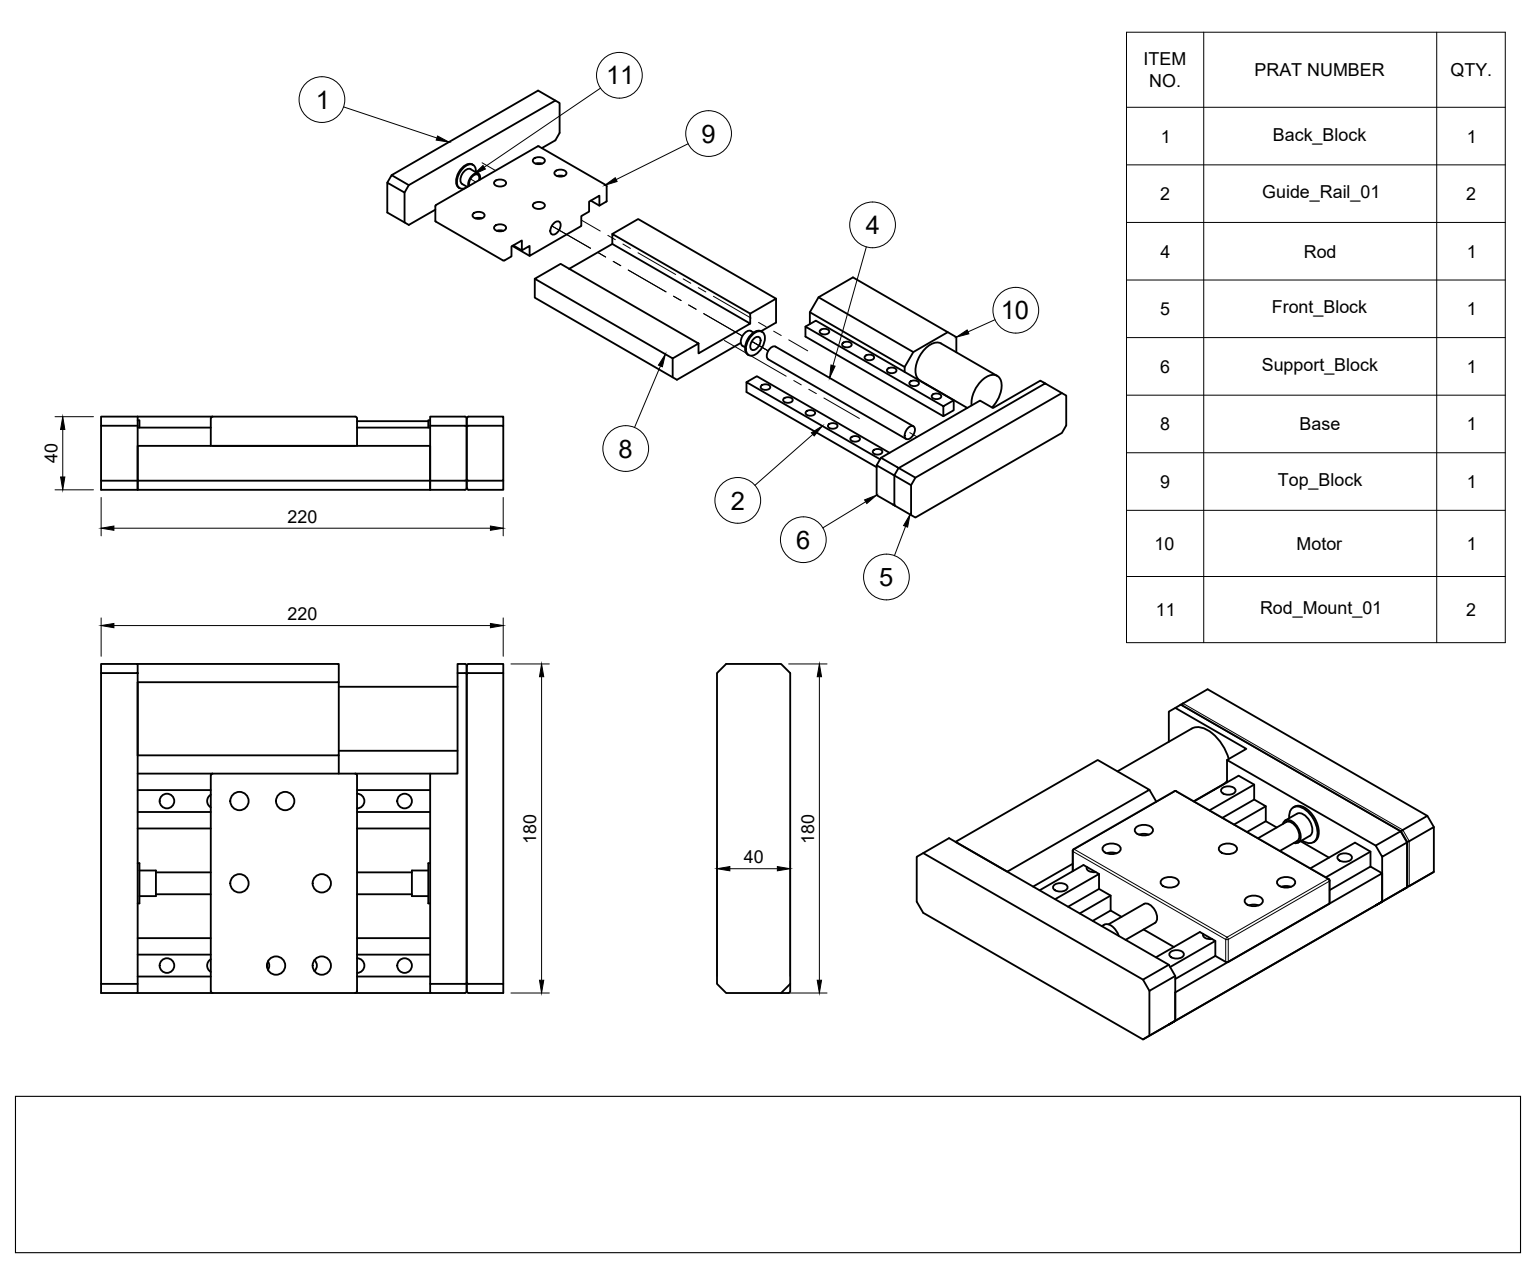
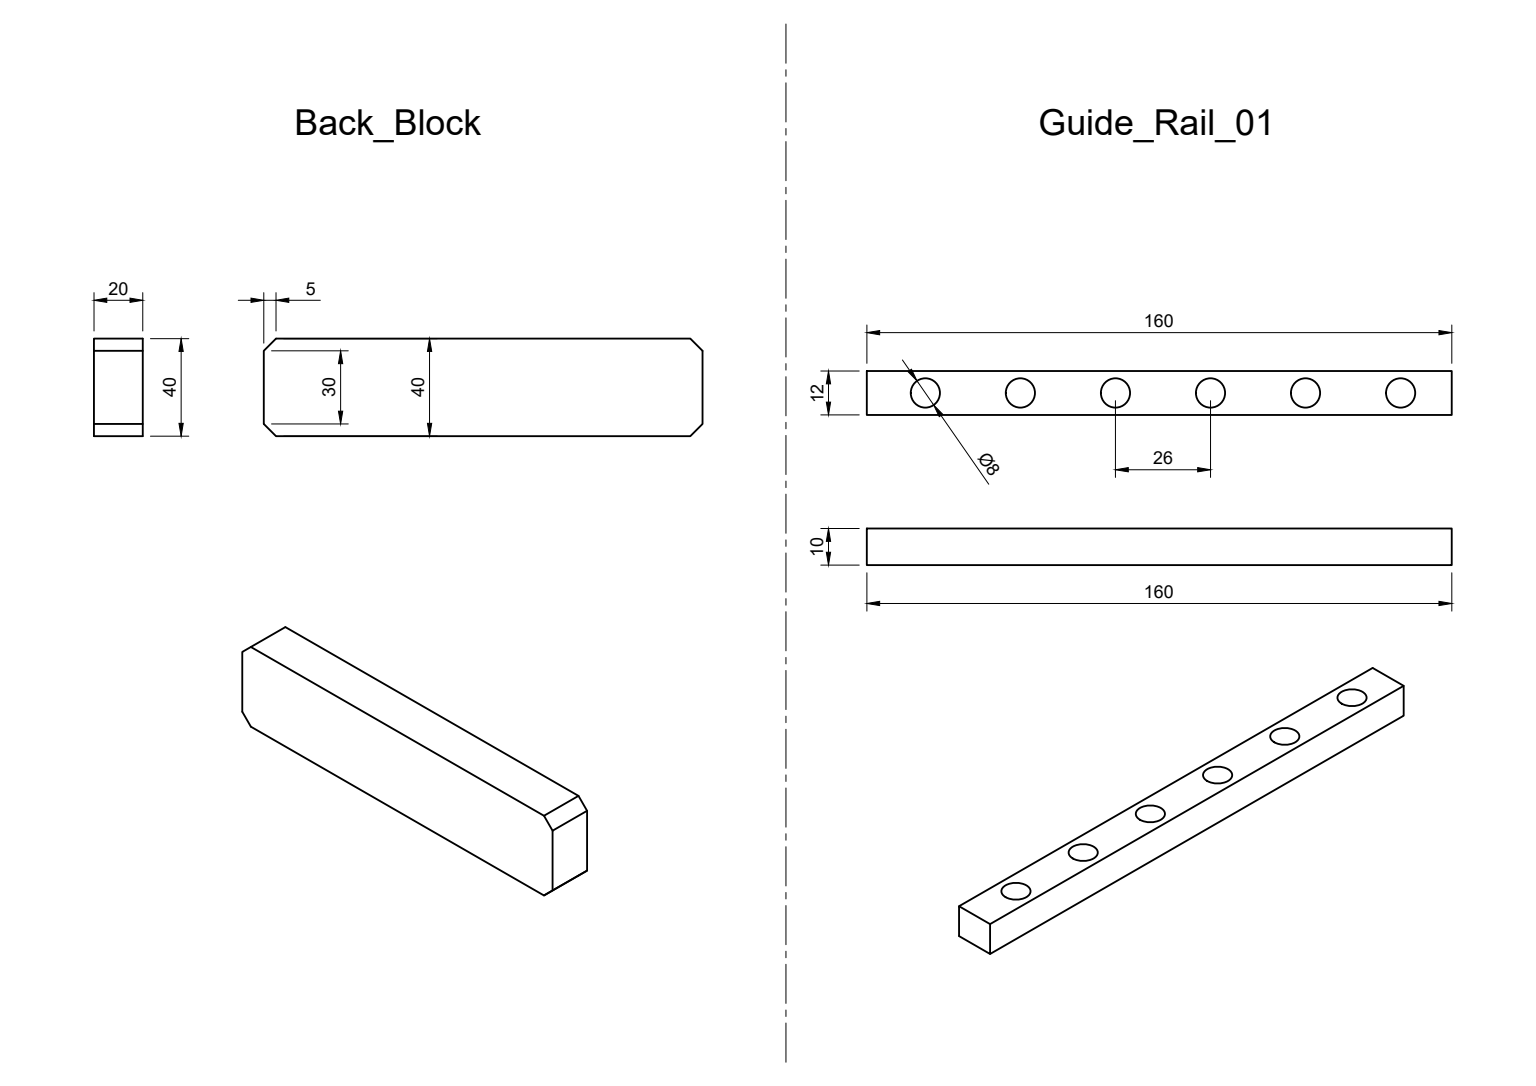
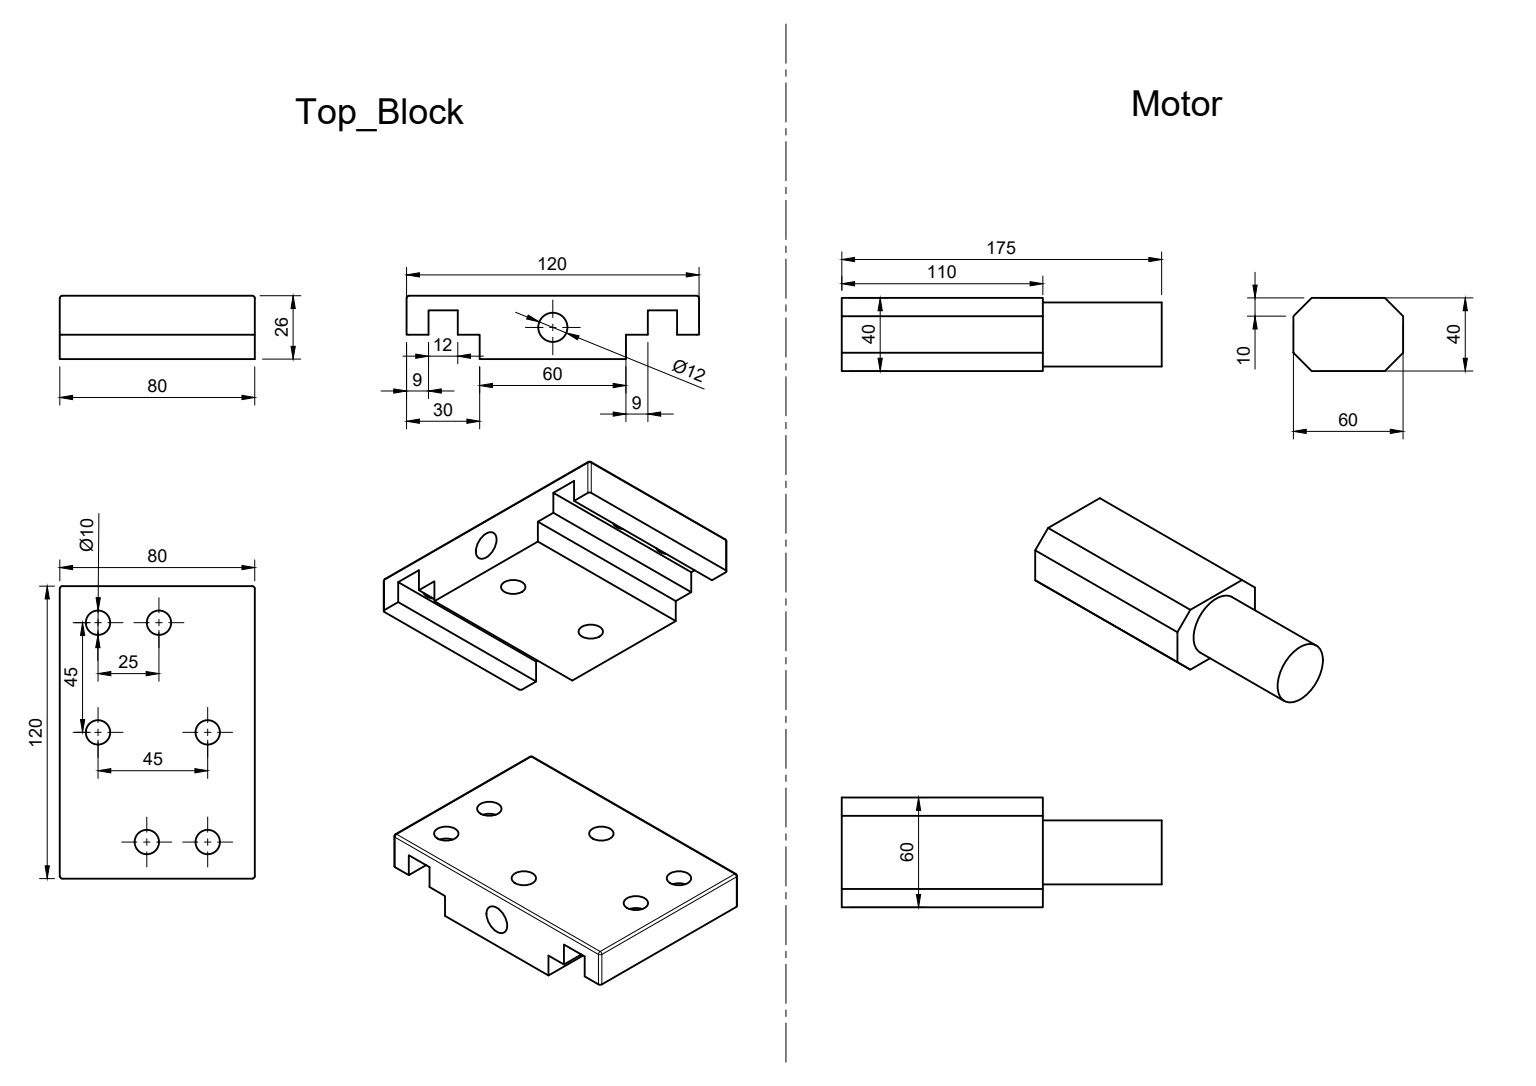
ISO-10303-21;
HEADER;
/* Generated by software containing ST-Developer
 * from STEP Tools, Inc. (www.steptools.com) 
 */

FILE_DESCRIPTION(
/* description */ (''),
/* implementation_level */ '2;1');

FILE_NAME(
/* name */ 'MAS-269',
/* time_stamp */ '2026-10-19T02:00:06+06:00',
/* author */ (''),
/* organization */ (''),
/* preprocessor_version */ 'ST-DEVELOPER v20.2',
/* originating_system */ 'Autodesk Translation Framework v15.15.0.0',
/* authorisation */ '');

FILE_SCHEMA (('AUTOMOTIVE_DESIGN { 1 0 10303 214 3 1 1 }'));
ENDSEC;

DATA;
#10=MECHANICAL_DESIGN_GEOMETRIC_PRESENTATION_REPRESENTATION('',(#105,#106,
#107,#108,#109,#110,#111,#112,#113,#114,#115),#4833);
#11=ITEM_DEFINED_TRANSFORMATION($,$,#2821,#3079);
#12=ITEM_DEFINED_TRANSFORMATION($,$,#2852,#3080);
#13=ITEM_DEFINED_TRANSFORMATION($,$,#2883,#3081);
#14=ITEM_DEFINED_TRANSFORMATION($,$,#2889,#3082);
#15=ITEM_DEFINED_TRANSFORMATION($,$,#2916,#3083);
#16=ITEM_DEFINED_TRANSFORMATION($,$,#2945,#3084);
#17=ITEM_DEFINED_TRANSFORMATION($,$,#2958,#3085);
#18=ITEM_DEFINED_TRANSFORMATION($,$,#2970,#3086);
#19=ITEM_DEFINED_TRANSFORMATION($,$,#3040,#3087);
#20=ITEM_DEFINED_TRANSFORMATION($,$,#3055,#3088);
#21=ITEM_DEFINED_TRANSFORMATION($,$,#3068,#3089);
#22=(
REPRESENTATION_RELATIONSHIP($,$,#4874,#4873)
REPRESENTATION_RELATIONSHIP_WITH_TRANSFORMATION(#11)
SHAPE_REPRESENTATION_RELATIONSHIP()
);
#23=(
REPRESENTATION_RELATIONSHIP($,$,#4875,#4873)
REPRESENTATION_RELATIONSHIP_WITH_TRANSFORMATION(#12)
SHAPE_REPRESENTATION_RELATIONSHIP()
);
#24=(
REPRESENTATION_RELATIONSHIP($,$,#4876,#4873)
REPRESENTATION_RELATIONSHIP_WITH_TRANSFORMATION(#13)
SHAPE_REPRESENTATION_RELATIONSHIP()
);
#25=(
REPRESENTATION_RELATIONSHIP($,$,#4877,#4873)
REPRESENTATION_RELATIONSHIP_WITH_TRANSFORMATION(#14)
SHAPE_REPRESENTATION_RELATIONSHIP()
);
#26=(
REPRESENTATION_RELATIONSHIP($,$,#4878,#4873)
REPRESENTATION_RELATIONSHIP_WITH_TRANSFORMATION(#15)
SHAPE_REPRESENTATION_RELATIONSHIP()
);
#27=(
REPRESENTATION_RELATIONSHIP($,$,#4879,#4873)
REPRESENTATION_RELATIONSHIP_WITH_TRANSFORMATION(#16)
SHAPE_REPRESENTATION_RELATIONSHIP()
);
#28=(
REPRESENTATION_RELATIONSHIP($,$,#4880,#4873)
REPRESENTATION_RELATIONSHIP_WITH_TRANSFORMATION(#17)
SHAPE_REPRESENTATION_RELATIONSHIP()
);
#29=(
REPRESENTATION_RELATIONSHIP($,$,#4881,#4873)
REPRESENTATION_RELATIONSHIP_WITH_TRANSFORMATION(#18)
SHAPE_REPRESENTATION_RELATIONSHIP()
);
#30=(
REPRESENTATION_RELATIONSHIP($,$,#4882,#4873)
REPRESENTATION_RELATIONSHIP_WITH_TRANSFORMATION(#19)
SHAPE_REPRESENTATION_RELATIONSHIP()
);
#31=(
REPRESENTATION_RELATIONSHIP($,$,#4883,#4873)
REPRESENTATION_RELATIONSHIP_WITH_TRANSFORMATION(#20)
SHAPE_REPRESENTATION_RELATIONSHIP()
);
#32=(
REPRESENTATION_RELATIONSHIP($,$,#4884,#4873)
REPRESENTATION_RELATIONSHIP_WITH_TRANSFORMATION(#21)
SHAPE_REPRESENTATION_RELATIONSHIP()
);
#33=CONTEXT_DEPENDENT_SHAPE_REPRESENTATION(#22,#4862);
#34=CONTEXT_DEPENDENT_SHAPE_REPRESENTATION(#23,#4863);
#35=CONTEXT_DEPENDENT_SHAPE_REPRESENTATION(#24,#4864);
#36=CONTEXT_DEPENDENT_SHAPE_REPRESENTATION(#25,#4865);
#37=CONTEXT_DEPENDENT_SHAPE_REPRESENTATION(#26,#4866);
#38=CONTEXT_DEPENDENT_SHAPE_REPRESENTATION(#27,#4867);
#39=CONTEXT_DEPENDENT_SHAPE_REPRESENTATION(#28,#4868);
#40=CONTEXT_DEPENDENT_SHAPE_REPRESENTATION(#29,#4869);
#41=CONTEXT_DEPENDENT_SHAPE_REPRESENTATION(#30,#4870);
#42=CONTEXT_DEPENDENT_SHAPE_REPRESENTATION(#31,#4871);
#43=CONTEXT_DEPENDENT_SHAPE_REPRESENTATION(#32,#4872);
#44=NEXT_ASSEMBLY_USAGE_OCCURRENCE('Guide_Rail_01:1','Guide_Rail_01:1',
'Guide_Rail_01:1',#4886,#4887,'Guide_Rail_01:1');
#45=NEXT_ASSEMBLY_USAGE_OCCURRENCE('Guide_Rail_02:1','Guide_Rail_02:1',
'Guide_Rail_02:1',#4886,#4888,'Guide_Rail_02:1');
#46=NEXT_ASSEMBLY_USAGE_OCCURRENCE('Rod:1','Rod:1','Rod:1',#4886,#4889,
'Rod:1');
#47=NEXT_ASSEMBLY_USAGE_OCCURRENCE('Front_Block:1','Front_Block:1',
'Front_Block:1',#4886,#4890,'Front_Block:1');
#48=NEXT_ASSEMBLY_USAGE_OCCURRENCE('Support_Block:1','Support_Block:1',
'Support_Block:1',#4886,#4891,'Support_Block:1');
#49=NEXT_ASSEMBLY_USAGE_OCCURRENCE('Rod_Mount_01:1','Rod_Mount_01:1',
'Rod_Mount_01:1',#4886,#4892,'Rod_Mount_01:1');
#50=NEXT_ASSEMBLY_USAGE_OCCURRENCE('Base:1','Base:1','Base:1',#4886,#4893,
'Base:1');
#51=NEXT_ASSEMBLY_USAGE_OCCURRENCE('Top_Block:1','Top_Block:1',
'Top_Block:1',#4886,#4894,'Top_Block:1');
#52=NEXT_ASSEMBLY_USAGE_OCCURRENCE('Motor:1','Motor:1','Motor:1',#4886,
#4895,'Motor:1');
#53=NEXT_ASSEMBLY_USAGE_OCCURRENCE('Rod_Mount_02:1','Rod_Mount_02:1',
'Rod_Mount_02:1',#4886,#4896,'Rod_Mount_02:1');
#54=NEXT_ASSEMBLY_USAGE_OCCURRENCE('Back_Block:1','Back_Block:1',
'Back_Block:1',#4886,#4897,'Back_Block:1');
#55=SPHERICAL_SURFACE('',#2991,1.00000000000001);
#56=SPHERICAL_SURFACE('',#2997,0.999999999999996);
#57=SPHERICAL_SURFACE('',#3003,0.999999999999996);
#58=SPHERICAL_SURFACE('',#3010,0.999999999999996);
#59=B_SPLINE_CURVE_WITH_KNOTS('',3,(#4296,#4297,#4298,#4299,#4300,#4301,
#4302,#4303,#4304,#4305,#4306,#4307),.UNSPECIFIED.,.F.,.F.,(4,2,2,2,2,4),
(0.,0.104126648162078,0.208253296324155,0.41650659264831,0.61629680537715,
0.81608701810599),.UNSPECIFIED.);
#60=B_SPLINE_CURVE_WITH_KNOTS('',3,(#4308,#4309,#4310,#4311,#4312,#4313,
#4314,#4315,#4316,#4317,#4318,#4319,#4320,#4321,#4322,#4323,#4324,#4325,
#4326,#4327,#4328,#4329,#4330,#4331,#4332,#4333,#4334,#4335,#4336,#4337,
#4338,#4339),.UNSPECIFIED.,.F.,.F.,(4,2,2,2,2,2,2,2,2,2,2,2,2,2,2,4),(0.81608701810599,
1.01587723083483,1.21566744356367,1.42392073988783,1.5280473880499,1.63217403621198,
1.73630068437406,1.84042733253614,2.04868062886029,2.24847084158913,2.44826105431797,
2.64805126704681,2.84784147977565,3.05609477609981,3.16022142426189,3.26434807242396),
 .UNSPECIFIED.);
#61=B_SPLINE_CURVE_WITH_KNOTS('',3,(#4343,#4344,#4345,#4346,#4347,#4348,
#4349,#4350,#4351,#4352,#4353,#4354,#4355,#4356,#4357,#4358,#4359,#4360,
#4361,#4362,#4363,#4364,#4365,#4366,#4367,#4368,#4369,#4370,#4371,#4372,
#4373,#4374),.UNSPECIFIED.,.F.,.F.,(4,2,2,2,2,2,2,2,2,2,2,2,2,2,2,4),(0.,
0.104126648162077,0.208253296324155,0.41650659264831,0.616296805377151,
0.816087018105991,1.01587723083483,1.21566744356367,1.42392073988783,1.52804738804991,
1.63217403621198,1.73630068437406,1.84042733253614,2.04868062886029,2.24847084158913,
2.44826105431797),.UNSPECIFIED.);
#62=B_SPLINE_CURVE_WITH_KNOTS('',3,(#4375,#4376,#4377,#4378,#4379,#4380,
#4381,#4382,#4383,#4384,#4385,#4386),.UNSPECIFIED.,.F.,.F.,(4,2,2,2,2,4),
(2.44826105431797,2.64805126704681,2.84784147977565,3.05609477609981,3.16022142426189,
3.26434807242396),.UNSPECIFIED.);
#63=B_SPLINE_CURVE_WITH_KNOTS('',3,(#4408,#4409,#4410,#4411,#4412,#4413,
#4414,#4415,#4416,#4417,#4418,#4419),.UNSPECIFIED.,.F.,.F.,(4,2,2,2,2,4),
(0.,0.104126648162077,0.208253296324155,0.416506592648309,0.61629680537715,
0.816087018105991),.UNSPECIFIED.);
#64=B_SPLINE_CURVE_WITH_KNOTS('',3,(#4420,#4421,#4422,#4423,#4424,#4425,
#4426,#4427,#4428,#4429,#4430,#4431,#4432,#4433,#4434,#4435,#4436,#4437,
#4438,#4439,#4440,#4441,#4442,#4443,#4444,#4445,#4446,#4447,#4448,#4449,
#4450,#4451),.UNSPECIFIED.,.F.,.F.,(4,2,2,2,2,2,2,2,2,2,2,2,2,2,2,4),(0.816087018105991,
1.01587723083483,1.21566744356367,1.42392073988783,1.5280473880499,1.63217403621198,
1.73630068437406,1.84042733253614,2.04868062886029,2.24847084158913,2.44826105431797,
2.64805126704681,2.84784147977565,3.05609477609981,3.16022142426189,3.26434807242396),
 .UNSPECIFIED.);
#65=B_SPLINE_CURVE_WITH_KNOTS('',3,(#4455,#4456,#4457,#4458,#4459,#4460,
#4461,#4462,#4463,#4464,#4465,#4466,#4467,#4468,#4469,#4470,#4471,#4472,
#4473,#4474,#4475,#4476,#4477,#4478,#4479,#4480,#4481,#4482,#4483,#4484,
#4485,#4486),.UNSPECIFIED.,.F.,.F.,(4,2,2,2,2,2,2,2,2,2,2,2,2,2,2,4),(0.,
0.104126648162077,0.208253296324155,0.416506592648309,0.61629680537715,
0.816087018105991,1.01587723083483,1.21566744356367,1.42392073988783,1.5280473880499,
1.63217403621198,1.73630068437406,1.84042733253614,2.04868062886029,2.24847084158913,
2.44826105431797),.UNSPECIFIED.);
#66=B_SPLINE_CURVE_WITH_KNOTS('',3,(#4487,#4488,#4489,#4490,#4491,#4492,
#4493,#4494,#4495,#4496,#4497,#4498),.UNSPECIFIED.,.F.,.F.,(4,2,2,2,2,4),
(2.44826105431797,2.64805126704681,2.84784147977565,3.05609477609981,3.16022142426189,
3.26434807242396),.UNSPECIFIED.);
#67=ELLIPSE('',#2891,1.08239220029239,1.);
#68=ELLIPSE('',#2892,1.08239220029239,1.);
#69=ELLIPSE('',#2894,1.08239220029239,1.);
#70=ELLIPSE('',#2896,1.08239220029239,1.);
#71=ELLIPSE('',#2898,1.08239220029239,1.);
#72=ELLIPSE('',#2899,1.08239220029239,1.);
#73=ELLIPSE('',#2901,1.0823922002924,1.);
#74=ELLIPSE('',#2904,1.08239220029239,1.);
#75=ELLIPSE('',#2918,1.08239220029239,1.);
#76=ELLIPSE('',#2919,1.0823922002924,1.);
#77=ELLIPSE('',#2921,1.08239220029239,1.);
#78=ELLIPSE('',#2923,1.08239220029239,1.);
#79=ELLIPSE('',#2924,1.0823922002924,1.);
#80=ELLIPSE('',#2927,1.0823922002924,1.);
#81=ELLIPSE('',#2929,1.08239220029239,1.);
#82=ELLIPSE('',#2931,1.08239220029239,1.);
#83=SHAPE_REPRESENTATION_RELATIONSHIP('SRR','None',#4874,#94);
#84=SHAPE_REPRESENTATION_RELATIONSHIP('SRR','None',#4875,#95);
#85=SHAPE_REPRESENTATION_RELATIONSHIP('SRR','None',#4876,#96);
#86=SHAPE_REPRESENTATION_RELATIONSHIP('SRR','None',#4877,#97);
#87=SHAPE_REPRESENTATION_RELATIONSHIP('SRR','None',#4878,#98);
#88=SHAPE_REPRESENTATION_RELATIONSHIP('SRR','None',#4879,#99);
#89=SHAPE_REPRESENTATION_RELATIONSHIP('SRR','None',#4880,#100);
#90=SHAPE_REPRESENTATION_RELATIONSHIP('SRR','None',#4881,#101);
#91=SHAPE_REPRESENTATION_RELATIONSHIP('SRR','None',#4882,#102);
#92=SHAPE_REPRESENTATION_RELATIONSHIP('SRR','None',#4883,#103);
#93=SHAPE_REPRESENTATION_RELATIONSHIP('SRR','None',#4884,#104);
#94=ADVANCED_BREP_SHAPE_REPRESENTATION('',(#116),#4822);
#95=ADVANCED_BREP_SHAPE_REPRESENTATION('',(#117),#4823);
#96=ADVANCED_BREP_SHAPE_REPRESENTATION('',(#118),#4824);
#97=ADVANCED_BREP_SHAPE_REPRESENTATION('',(#119),#4825);
#98=ADVANCED_BREP_SHAPE_REPRESENTATION('',(#120),#4826);
#99=ADVANCED_BREP_SHAPE_REPRESENTATION('',(#121),#4827);
#100=ADVANCED_BREP_SHAPE_REPRESENTATION('',(#122),#4828);
#101=ADVANCED_BREP_SHAPE_REPRESENTATION('',(#123),#4829);
#102=ADVANCED_BREP_SHAPE_REPRESENTATION('',(#124),#4830);
#103=ADVANCED_BREP_SHAPE_REPRESENTATION('',(#125),#4831);
#104=ADVANCED_BREP_SHAPE_REPRESENTATION('',(#126),#4832);
#105=STYLED_ITEM('',(#5006),#116);
#106=STYLED_ITEM('',(#5006),#117);
#107=STYLED_ITEM('',(#4992),#118);
#108=STYLED_ITEM('',(#4971),#119);
#109=STYLED_ITEM('',(#4971),#120);
#110=STYLED_ITEM('',(#4992),#121);
#111=STYLED_ITEM('',(#4971),#122);
#112=STYLED_ITEM('',(#4971),#123);
#113=STYLED_ITEM('',(#5006),#124);
#114=STYLED_ITEM('',(#4992),#125);
#115=STYLED_ITEM('',(#4971),#126);
#116=MANIFOLD_SOLID_BREP('Guide_Rail_01',#2687);
#117=MANIFOLD_SOLID_BREP('Guide_Rail_02',#2688);
#118=MANIFOLD_SOLID_BREP('Rod',#2689);
#119=MANIFOLD_SOLID_BREP('Front_Block',#2690);
#120=MANIFOLD_SOLID_BREP('Support_Block',#2691);
#121=MANIFOLD_SOLID_BREP('Rod_Mount_01',#2692);
#122=MANIFOLD_SOLID_BREP('Base',#2693);
#123=MANIFOLD_SOLID_BREP('Body1',#2694);
#124=MANIFOLD_SOLID_BREP('Motor',#2695);
#125=MANIFOLD_SOLID_BREP('Rod_Mount_02',#2696);
#126=MANIFOLD_SOLID_BREP('Back_Block',#2697);
#127=FACE_BOUND('',#446,.T.);
#128=FACE_BOUND('',#447,.T.);
#129=FACE_BOUND('',#448,.T.);
#130=FACE_BOUND('',#449,.T.);
#131=FACE_BOUND('',#450,.T.);
#132=FACE_BOUND('',#451,.T.);
#133=FACE_BOUND('',#470,.T.);
#134=FACE_BOUND('',#471,.T.);
#135=FACE_BOUND('',#472,.T.);
#136=FACE_BOUND('',#473,.T.);
#137=FACE_BOUND('',#474,.T.);
#138=FACE_BOUND('',#475,.T.);
#139=FACE_BOUND('',#521,.T.);
#140=FACE_BOUND('',#524,.T.);
#141=FACE_BOUND('',#526,.T.);
#142=FACE_BOUND('',#559,.T.);
#143=FACE_BOUND('',#563,.T.);
#144=FACE_BOUND('',#564,.T.);
#145=FACE_BOUND('',#565,.T.);
#146=FACE_BOUND('',#566,.T.);
#147=FACE_BOUND('',#567,.T.);
#148=FACE_BOUND('',#568,.T.);
#149=FACE_BOUND('',#570,.T.);
#150=FACE_BOUND('',#571,.T.);
#151=FACE_BOUND('',#572,.T.);
#152=FACE_BOUND('',#573,.T.);
#153=FACE_BOUND('',#577,.T.);
#154=FACE_BOUND('',#578,.T.);
#155=FACE_BOUND('',#582,.T.);
#156=FACE_BOUND('',#583,.T.);
#157=FACE_BOUND('',#590,.T.);
#158=FACE_BOUND('',#592,.T.);
#159=FACE_BOUND('',#593,.T.);
#160=FACE_BOUND('',#607,.T.);
#161=FACE_BOUND('',#611,.T.);
#162=FACE_BOUND('',#614,.T.);
#163=FACE_BOUND('',#616,.T.);
#164=PLANE('',#2825);
#165=PLANE('',#2829);
#166=PLANE('',#2833);
#167=PLANE('',#2837);
#168=PLANE('',#2841);
#169=PLANE('',#2845);
#170=PLANE('',#2846);
#171=PLANE('',#2847);
#172=PLANE('',#2848);
#173=PLANE('',#2849);
#174=PLANE('',#2850);
#175=PLANE('',#2851);
#176=PLANE('',#2856);
#177=PLANE('',#2860);
#178=PLANE('',#2864);
#179=PLANE('',#2868);
#180=PLANE('',#2872);
#181=PLANE('',#2876);
#182=PLANE('',#2877);
#183=PLANE('',#2878);
#184=PLANE('',#2879);
#185=PLANE('',#2880);
#186=PLANE('',#2881);
#187=PLANE('',#2882);
#188=PLANE('',#2887);
#189=PLANE('',#2888);
#190=PLANE('',#2906);
#191=PLANE('',#2907);
#192=PLANE('',#2908);
#193=PLANE('',#2909);
#194=PLANE('',#2910);
#195=PLANE('',#2911);
#196=PLANE('',#2912);
#197=PLANE('',#2913);
#198=PLANE('',#2914);
#199=PLANE('',#2915);
#200=PLANE('',#2933);
#201=PLANE('',#2934);
#202=PLANE('',#2935);
#203=PLANE('',#2936);
#204=PLANE('',#2937);
#205=PLANE('',#2938);
#206=PLANE('',#2939);
#207=PLANE('',#2940);
#208=PLANE('',#2941);
#209=PLANE('',#2942);
#210=PLANE('',#2943);
#211=PLANE('',#2944);
#212=PLANE('',#2952);
#213=PLANE('',#2956);
#214=PLANE('',#2957);
#215=PLANE('',#2959);
#216=PLANE('',#2960);
#217=PLANE('',#2961);
#218=PLANE('',#2962);
#219=PLANE('',#2963);
#220=PLANE('',#2964);
#221=PLANE('',#2965);
#222=PLANE('',#2966);
#223=PLANE('',#2967);
#224=PLANE('',#2968);
#225=PLANE('',#2969);
#226=PLANE('',#3019);
#227=PLANE('',#3021);
#228=PLANE('',#3022);
#229=PLANE('',#3023);
#230=PLANE('',#3026);
#231=PLANE('',#3027);
#232=PLANE('',#3028);
#233=PLANE('',#3029);
#234=PLANE('',#3030);
#235=PLANE('',#3031);
#236=PLANE('',#3032);
#237=PLANE('',#3033);
#238=PLANE('',#3034);
#239=PLANE('',#3035);
#240=PLANE('',#3036);
#241=PLANE('',#3037);
#242=PLANE('',#3038);
#243=PLANE('',#3039);
#244=PLANE('',#3044);
#245=PLANE('',#3045);
#246=PLANE('',#3046);
#247=PLANE('',#3047);
#248=PLANE('',#3048);
#249=PLANE('',#3049);
#250=PLANE('',#3050);
#251=PLANE('',#3051);
#252=PLANE('',#3052);
#253=PLANE('',#3053);
#254=PLANE('',#3054);
#255=PLANE('',#3062);
#256=PLANE('',#3066);
#257=PLANE('',#3067);
#258=PLANE('',#3069);
#259=PLANE('',#3070);
#260=PLANE('',#3071);
#261=PLANE('',#3072);
#262=PLANE('',#3073);
#263=PLANE('',#3074);
#264=PLANE('',#3075);
#265=PLANE('',#3076);
#266=PLANE('',#3077);
#267=PLANE('',#3078);
#268=FACE_OUTER_BOUND('',#429,.T.);
#269=FACE_OUTER_BOUND('',#430,.T.);
#270=FACE_OUTER_BOUND('',#431,.T.);
#271=FACE_OUTER_BOUND('',#432,.T.);
#272=FACE_OUTER_BOUND('',#433,.T.);
#273=FACE_OUTER_BOUND('',#434,.T.);
#274=FACE_OUTER_BOUND('',#435,.T.);
#275=FACE_OUTER_BOUND('',#436,.T.);
#276=FACE_OUTER_BOUND('',#437,.T.);
#277=FACE_OUTER_BOUND('',#438,.T.);
#278=FACE_OUTER_BOUND('',#439,.T.);
#279=FACE_OUTER_BOUND('',#440,.T.);
#280=FACE_OUTER_BOUND('',#441,.T.);
#281=FACE_OUTER_BOUND('',#442,.T.);
#282=FACE_OUTER_BOUND('',#443,.T.);
#283=FACE_OUTER_BOUND('',#444,.T.);
#284=FACE_OUTER_BOUND('',#445,.T.);
#285=FACE_OUTER_BOUND('',#452,.T.);
#286=FACE_OUTER_BOUND('',#453,.T.);
#287=FACE_OUTER_BOUND('',#454,.T.);
#288=FACE_OUTER_BOUND('',#455,.T.);
#289=FACE_OUTER_BOUND('',#456,.T.);
#290=FACE_OUTER_BOUND('',#457,.T.);
#291=FACE_OUTER_BOUND('',#458,.T.);
#292=FACE_OUTER_BOUND('',#459,.T.);
#293=FACE_OUTER_BOUND('',#460,.T.);
#294=FACE_OUTER_BOUND('',#461,.T.);
#295=FACE_OUTER_BOUND('',#462,.T.);
#296=FACE_OUTER_BOUND('',#463,.T.);
#297=FACE_OUTER_BOUND('',#464,.T.);
#298=FACE_OUTER_BOUND('',#465,.T.);
#299=FACE_OUTER_BOUND('',#466,.T.);
#300=FACE_OUTER_BOUND('',#467,.T.);
#301=FACE_OUTER_BOUND('',#468,.T.);
#302=FACE_OUTER_BOUND('',#469,.T.);
#303=FACE_OUTER_BOUND('',#476,.T.);
#304=FACE_OUTER_BOUND('',#477,.T.);
#305=FACE_OUTER_BOUND('',#478,.T.);
#306=FACE_OUTER_BOUND('',#479,.T.);
#307=FACE_OUTER_BOUND('',#480,.T.);
#308=FACE_OUTER_BOUND('',#481,.T.);
#309=FACE_OUTER_BOUND('',#482,.T.);
#310=FACE_OUTER_BOUND('',#483,.T.);
#311=FACE_OUTER_BOUND('',#484,.T.);
#312=FACE_OUTER_BOUND('',#485,.T.);
#313=FACE_OUTER_BOUND('',#486,.T.);
#314=FACE_OUTER_BOUND('',#487,.T.);
#315=FACE_OUTER_BOUND('',#488,.T.);
#316=FACE_OUTER_BOUND('',#489,.T.);
#317=FACE_OUTER_BOUND('',#490,.T.);
#318=FACE_OUTER_BOUND('',#491,.T.);
#319=FACE_OUTER_BOUND('',#492,.T.);
#320=FACE_OUTER_BOUND('',#493,.T.);
#321=FACE_OUTER_BOUND('',#494,.T.);
#322=FACE_OUTER_BOUND('',#495,.T.);
#323=FACE_OUTER_BOUND('',#496,.T.);
#324=FACE_OUTER_BOUND('',#497,.T.);
#325=FACE_OUTER_BOUND('',#498,.T.);
#326=FACE_OUTER_BOUND('',#499,.T.);
#327=FACE_OUTER_BOUND('',#500,.T.);
#328=FACE_OUTER_BOUND('',#501,.T.);
#329=FACE_OUTER_BOUND('',#502,.T.);
#330=FACE_OUTER_BOUND('',#503,.T.);
#331=FACE_OUTER_BOUND('',#504,.T.);
#332=FACE_OUTER_BOUND('',#505,.T.);
#333=FACE_OUTER_BOUND('',#506,.T.);
#334=FACE_OUTER_BOUND('',#507,.T.);
#335=FACE_OUTER_BOUND('',#508,.T.);
#336=FACE_OUTER_BOUND('',#509,.T.);
#337=FACE_OUTER_BOUND('',#510,.T.);
#338=FACE_OUTER_BOUND('',#511,.T.);
#339=FACE_OUTER_BOUND('',#512,.T.);
#340=FACE_OUTER_BOUND('',#513,.T.);
#341=FACE_OUTER_BOUND('',#514,.T.);
#342=FACE_OUTER_BOUND('',#515,.T.);
#343=FACE_OUTER_BOUND('',#516,.T.);
#344=FACE_OUTER_BOUND('',#517,.T.);
#345=FACE_OUTER_BOUND('',#518,.T.);
#346=FACE_OUTER_BOUND('',#519,.T.);
#347=FACE_OUTER_BOUND('',#520,.T.);
#348=FACE_OUTER_BOUND('',#522,.T.);
#349=FACE_OUTER_BOUND('',#523,.T.);
#350=FACE_OUTER_BOUND('',#525,.T.);
#351=FACE_OUTER_BOUND('',#527,.T.);
#352=FACE_OUTER_BOUND('',#528,.T.);
#353=FACE_OUTER_BOUND('',#529,.T.);
#354=FACE_OUTER_BOUND('',#530,.T.);
#355=FACE_OUTER_BOUND('',#531,.T.);
#356=FACE_OUTER_BOUND('',#532,.T.);
#357=FACE_OUTER_BOUND('',#533,.T.);
#358=FACE_OUTER_BOUND('',#534,.T.);
#359=FACE_OUTER_BOUND('',#535,.T.);
#360=FACE_OUTER_BOUND('',#536,.T.);
#361=FACE_OUTER_BOUND('',#537,.T.);
#362=FACE_OUTER_BOUND('',#538,.T.);
#363=FACE_OUTER_BOUND('',#539,.T.);
#364=FACE_OUTER_BOUND('',#540,.T.);
#365=FACE_OUTER_BOUND('',#541,.T.);
#366=FACE_OUTER_BOUND('',#542,.T.);
#367=FACE_OUTER_BOUND('',#543,.T.);
#368=FACE_OUTER_BOUND('',#544,.T.);
#369=FACE_OUTER_BOUND('',#545,.T.);
#370=FACE_OUTER_BOUND('',#546,.T.);
#371=FACE_OUTER_BOUND('',#547,.T.);
#372=FACE_OUTER_BOUND('',#548,.T.);
#373=FACE_OUTER_BOUND('',#549,.T.);
#374=FACE_OUTER_BOUND('',#550,.T.);
#375=FACE_OUTER_BOUND('',#551,.T.);
#376=FACE_OUTER_BOUND('',#552,.T.);
#377=FACE_OUTER_BOUND('',#553,.T.);
#378=FACE_OUTER_BOUND('',#554,.T.);
#379=FACE_OUTER_BOUND('',#555,.T.);
#380=FACE_OUTER_BOUND('',#556,.T.);
#381=FACE_OUTER_BOUND('',#557,.T.);
#382=FACE_OUTER_BOUND('',#558,.T.);
#383=FACE_OUTER_BOUND('',#560,.T.);
#384=FACE_OUTER_BOUND('',#561,.T.);
#385=FACE_OUTER_BOUND('',#562,.T.);
#386=FACE_OUTER_BOUND('',#569,.T.);
#387=FACE_OUTER_BOUND('',#574,.T.);
#388=FACE_OUTER_BOUND('',#575,.T.);
#389=FACE_OUTER_BOUND('',#576,.T.);
#390=FACE_OUTER_BOUND('',#579,.T.);
#391=FACE_OUTER_BOUND('',#580,.T.);
#392=FACE_OUTER_BOUND('',#581,.T.);
#393=FACE_OUTER_BOUND('',#584,.T.);
#394=FACE_OUTER_BOUND('',#585,.T.);
#395=FACE_OUTER_BOUND('',#586,.T.);
#396=FACE_OUTER_BOUND('',#587,.T.);
#397=FACE_OUTER_BOUND('',#588,.T.);
#398=FACE_OUTER_BOUND('',#589,.T.);
#399=FACE_OUTER_BOUND('',#591,.T.);
#400=FACE_OUTER_BOUND('',#594,.T.);
#401=FACE_OUTER_BOUND('',#595,.T.);
#402=FACE_OUTER_BOUND('',#596,.T.);
#403=FACE_OUTER_BOUND('',#597,.T.);
#404=FACE_OUTER_BOUND('',#598,.T.);
#405=FACE_OUTER_BOUND('',#599,.T.);
#406=FACE_OUTER_BOUND('',#600,.T.);
#407=FACE_OUTER_BOUND('',#601,.T.);
#408=FACE_OUTER_BOUND('',#602,.T.);
#409=FACE_OUTER_BOUND('',#603,.T.);
#410=FACE_OUTER_BOUND('',#604,.T.);
#411=FACE_OUTER_BOUND('',#605,.T.);
#412=FACE_OUTER_BOUND('',#606,.T.);
#413=FACE_OUTER_BOUND('',#608,.T.);
#414=FACE_OUTER_BOUND('',#609,.T.);
#415=FACE_OUTER_BOUND('',#610,.T.);
#416=FACE_OUTER_BOUND('',#612,.T.);
#417=FACE_OUTER_BOUND('',#613,.T.);
#418=FACE_OUTER_BOUND('',#615,.T.);
#419=FACE_OUTER_BOUND('',#617,.T.);
#420=FACE_OUTER_BOUND('',#618,.T.);
#421=FACE_OUTER_BOUND('',#619,.T.);
#422=FACE_OUTER_BOUND('',#620,.T.);
#423=FACE_OUTER_BOUND('',#621,.T.);
#424=FACE_OUTER_BOUND('',#622,.T.);
#425=FACE_OUTER_BOUND('',#623,.T.);
#426=FACE_OUTER_BOUND('',#624,.T.);
#427=FACE_OUTER_BOUND('',#625,.T.);
#428=FACE_OUTER_BOUND('',#626,.T.);
#429=EDGE_LOOP('',(#1777,#1778,#1779,#1780));
#430=EDGE_LOOP('',(#1781));
#431=EDGE_LOOP('',(#1782,#1783,#1784,#1785));
#432=EDGE_LOOP('',(#1786));
#433=EDGE_LOOP('',(#1787,#1788,#1789,#1790));
#434=EDGE_LOOP('',(#1791));
#435=EDGE_LOOP('',(#1792,#1793,#1794,#1795));
#436=EDGE_LOOP('',(#1796));
#437=EDGE_LOOP('',(#1797,#1798,#1799,#1800));
#438=EDGE_LOOP('',(#1801));
#439=EDGE_LOOP('',(#1802,#1803,#1804,#1805));
#440=EDGE_LOOP('',(#1806));
#441=EDGE_LOOP('',(#1807,#1808,#1809,#1810));
#442=EDGE_LOOP('',(#1811,#1812,#1813,#1814));
#443=EDGE_LOOP('',(#1815,#1816,#1817,#1818));
#444=EDGE_LOOP('',(#1819,#1820,#1821,#1822));
#445=EDGE_LOOP('',(#1823,#1824,#1825,#1826));
#446=EDGE_LOOP('',(#1827));
#447=EDGE_LOOP('',(#1828));
#448=EDGE_LOOP('',(#1829));
#449=EDGE_LOOP('',(#1830));
#450=EDGE_LOOP('',(#1831));
#451=EDGE_LOOP('',(#1832));
#452=EDGE_LOOP('',(#1833,#1834,#1835,#1836));
#453=EDGE_LOOP('',(#1837,#1838,#1839,#1840));
#454=EDGE_LOOP('',(#1841));
#455=EDGE_LOOP('',(#1842,#1843,#1844,#1845));
#456=EDGE_LOOP('',(#1846));
#457=EDGE_LOOP('',(#1847,#1848,#1849,#1850));
#458=EDGE_LOOP('',(#1851));
#459=EDGE_LOOP('',(#1852,#1853,#1854,#1855));
#460=EDGE_LOOP('',(#1856));
#461=EDGE_LOOP('',(#1857,#1858,#1859,#1860));
#462=EDGE_LOOP('',(#1861));
#463=EDGE_LOOP('',(#1862,#1863,#1864,#1865));
#464=EDGE_LOOP('',(#1866));
#465=EDGE_LOOP('',(#1867,#1868,#1869,#1870));
#466=EDGE_LOOP('',(#1871,#1872,#1873,#1874));
#467=EDGE_LOOP('',(#1875,#1876,#1877,#1878));
#468=EDGE_LOOP('',(#1879,#1880,#1881,#1882));
#469=EDGE_LOOP('',(#1883,#1884,#1885,#1886));
#470=EDGE_LOOP('',(#1887));
#471=EDGE_LOOP('',(#1888));
#472=EDGE_LOOP('',(#1889));
#473=EDGE_LOOP('',(#1890));
#474=EDGE_LOOP('',(#1891));
#475=EDGE_LOOP('',(#1892));
#476=EDGE_LOOP('',(#1893,#1894,#1895,#1896));
#477=EDGE_LOOP('',(#1897,#1898,#1899,#1900));
#478=EDGE_LOOP('',(#1901));
#479=EDGE_LOOP('',(#1902));
#480=EDGE_LOOP('',(#1903,#1904,#1905,#1906));
#481=EDGE_LOOP('',(#1907,#1908,#1909,#1910));
#482=EDGE_LOOP('',(#1911,#1912,#1913,#1914));
#483=EDGE_LOOP('',(#1915,#1916,#1917,#1918));
#484=EDGE_LOOP('',(#1919,#1920,#1921,#1922));
#485=EDGE_LOOP('',(#1923,#1924,#1925,#1926));
#486=EDGE_LOOP('',(#1927,#1928,#1929,#1930));
#487=EDGE_LOOP('',(#1931,#1932,#1933,#1934));
#488=EDGE_LOOP('',(#1935,#1936,#1937,#1938));
#489=EDGE_LOOP('',(#1939,#1940,#1941,#1942));
#490=EDGE_LOOP('',(#1943,#1944,#1945,#1946));
#491=EDGE_LOOP('',(#1947,#1948,#1949,#1950));
#492=EDGE_LOOP('',(#1951,#1952,#1953,#1954,#1955,#1956,#1957,#1958));
#493=EDGE_LOOP('',(#1959,#1960,#1961,#1962));
#494=EDGE_LOOP('',(#1963,#1964,#1965,#1966));
#495=EDGE_LOOP('',(#1967,#1968,#1969,#1970));
#496=EDGE_LOOP('',(#1971,#1972,#1973,#1974));
#497=EDGE_LOOP('',(#1975,#1976,#1977,#1978,#1979,#1980,#1981,#1982));
#498=EDGE_LOOP('',(#1983,#1984,#1985,#1986));
#499=EDGE_LOOP('',(#1987,#1988,#1989,#1990));
#500=EDGE_LOOP('',(#1991,#1992,#1993,#1994));
#501=EDGE_LOOP('',(#1995,#1996,#1997,#1998));
#502=EDGE_LOOP('',(#1999,#2000,#2001,#2002));
#503=EDGE_LOOP('',(#2003,#2004,#2005,#2006));
#504=EDGE_LOOP('',(#2007,#2008,#2009,#2010));
#505=EDGE_LOOP('',(#2011,#2012,#2013,#2014));
#506=EDGE_LOOP('',(#2015,#2016,#2017,#2018));
#507=EDGE_LOOP('',(#2019,#2020,#2021,#2022,#2023,#2024));
#508=EDGE_LOOP('',(#2025,#2026,#2027,#2028));
#509=EDGE_LOOP('',(#2029,#2030,#2031,#2032));
#510=EDGE_LOOP('',(#2033,#2034,#2035,#2036,#2037,#2038,#2039,#2040));
#511=EDGE_LOOP('',(#2041,#2042,#2043,#2044));
#512=EDGE_LOOP('',(#2045,#2046,#2047,#2048,#2049,#2050));
#513=EDGE_LOOP('',(#2051,#2052,#2053,#2054));
#514=EDGE_LOOP('',(#2055,#2056,#2057,#2058));
#515=EDGE_LOOP('',(#2059,#2060,#2061,#2062));
#516=EDGE_LOOP('',(#2063,#2064,#2065,#2066,#2067,#2068));
#517=EDGE_LOOP('',(#2069,#2070,#2071,#2072,#2073,#2074));
#518=EDGE_LOOP('',(#2075,#2076,#2077,#2078));
#519=EDGE_LOOP('',(#2079,#2080,#2081,#2082));
#520=EDGE_LOOP('',(#2083));
#521=EDGE_LOOP('',(#2084));
#522=EDGE_LOOP('',(#2085,#2086,#2087,#2088));
#523=EDGE_LOOP('',(#2089));
#524=EDGE_LOOP('',(#2090));
#525=EDGE_LOOP('',(#2091));
#526=EDGE_LOOP('',(#2092));
#527=EDGE_LOOP('',(#2093,#2094,#2095,#2096));
#528=EDGE_LOOP('',(#2097,#2098,#2099,#2100));
#529=EDGE_LOOP('',(#2101,#2102,#2103,#2104));
#530=EDGE_LOOP('',(#2105,#2106,#2107,#2108));
#531=EDGE_LOOP('',(#2109,#2110,#2111,#2112));
#532=EDGE_LOOP('',(#2113,#2114,#2115,#2116));
#533=EDGE_LOOP('',(#2117,#2118,#2119,#2120));
#534=EDGE_LOOP('',(#2121,#2122,#2123,#2124));
#535=EDGE_LOOP('',(#2125,#2126,#2127,#2128));
#536=EDGE_LOOP('',(#2129,#2130,#2131,#2132,#2133,#2134,#2135,#2136,#2137));
#537=EDGE_LOOP('',(#2138,#2139,#2140,#2141,#2142,#2143,#2144,#2145,#2146));
#538=EDGE_LOOP('',(#2147,#2148,#2149,#2150,#2151));
#539=EDGE_LOOP('',(#2152,#2153,#2154,#2155,#2156));
#540=EDGE_LOOP('',(#2157,#2158,#2159,#2160));
#541=EDGE_LOOP('',(#2161,#2162,#2163,#2164));
#542=EDGE_LOOP('',(#2165,#2166,#2167,#2168,#2169));
#543=EDGE_LOOP('',(#2170,#2171,#2172,#2173,#2174));
#544=EDGE_LOOP('',(#2175,#2176,#2177,#2178));
#545=EDGE_LOOP('',(#2179,#2180,#2181,#2182));
#546=EDGE_LOOP('',(#2183,#2184,#2185));
#547=EDGE_LOOP('',(#2186,#2187,#2188,#2189));
#548=EDGE_LOOP('',(#2190,#2191,#2192));
#549=EDGE_LOOP('',(#2193,#2194,#2195,#2196));
#550=EDGE_LOOP('',(#2197,#2198,#2199));
#551=EDGE_LOOP('',(#2200,#2201,#2202,#2203));
#552=EDGE_LOOP('',(#2204,#2205,#2206,#2207));
#553=EDGE_LOOP('',(#2208,#2209,#2210));
#554=EDGE_LOOP('',(#2211,#2212,#2213,#2214));
#555=EDGE_LOOP('',(#2215,#2216,#2217,#2218));
#556=EDGE_LOOP('',(#2219,#2220,#2221,#2222));
#557=EDGE_LOOP('',(#2223,#2224,#2225,#2226));
#558=EDGE_LOOP('',(#2227,#2228,#2229,#2230,#2231,#2232,#2233,#2234,#2235,
#2236,#2237,#2238,#2239,#2240,#2241,#2242));
#559=EDGE_LOOP('',(#2243));
#560=EDGE_LOOP('',(#2244,#2245,#2246,#2247));
#561=EDGE_LOOP('',(#2248,#2249,#2250,#2251,#2252,#2253));
#562=EDGE_LOOP('',(#2254,#2255,#2256,#2257));
#563=EDGE_LOOP('',(#2258));
#564=EDGE_LOOP('',(#2259));
#565=EDGE_LOOP('',(#2260));
#566=EDGE_LOOP('',(#2261));
#567=EDGE_LOOP('',(#2262));
#568=EDGE_LOOP('',(#2263));
#569=EDGE_LOOP('',(#2264,#2265,#2266,#2267));
#570=EDGE_LOOP('',(#2268,#2269));
#571=EDGE_LOOP('',(#2270,#2271));
#572=EDGE_LOOP('',(#2272,#2273));
#573=EDGE_LOOP('',(#2274,#2275));
#574=EDGE_LOOP('',(#2276,#2277,#2278,#2279));
#575=EDGE_LOOP('',(#2280,#2281,#2282,#2283));
#576=EDGE_LOOP('',(#2284,#2285,#2286,#2287));
#577=EDGE_LOOP('',(#2288));
#578=EDGE_LOOP('',(#2289));
#579=EDGE_LOOP('',(#2290,#2291,#2292,#2293));
#580=EDGE_LOOP('',(#2294,#2295,#2296,#2297));
#581=EDGE_LOOP('',(#2298,#2299,#2300,#2301));
#582=EDGE_LOOP('',(#2302));
#583=EDGE_LOOP('',(#2303));
#584=EDGE_LOOP('',(#2304,#2305,#2306,#2307,#2308,#2309));
#585=EDGE_LOOP('',(#2310,#2311,#2312,#2313));
#586=EDGE_LOOP('',(#2314,#2315,#2316,#2317));
#587=EDGE_LOOP('',(#2318,#2319,#2320,#2321));
#588=EDGE_LOOP('',(#2322,#2323,#2324,#2325));
#589=EDGE_LOOP('',(#2326,#2327,#2328,#2329,#2330,#2331,#2332,#2333,#2334,
#2335,#2336,#2337,#2338,#2339,#2340,#2341));
#590=EDGE_LOOP('',(#2342));
#591=EDGE_LOOP('',(#2343,#2344,#2345,#2346));
#592=EDGE_LOOP('',(#2347));
#593=EDGE_LOOP('',(#2348));
#594=EDGE_LOOP('',(#2349,#2350,#2351,#2352));
#595=EDGE_LOOP('',(#2353,#2354,#2355,#2356));
#596=EDGE_LOOP('',(#2357));
#597=EDGE_LOOP('',(#2358,#2359,#2360,#2361));
#598=EDGE_LOOP('',(#2362,#2363,#2364,#2365,#2366,#2367,#2368,#2369));
#599=EDGE_LOOP('',(#2370,#2371,#2372,#2373));
#600=EDGE_LOOP('',(#2374,#2375,#2376,#2377));
#601=EDGE_LOOP('',(#2378,#2379,#2380,#2381));
#602=EDGE_LOOP('',(#2382,#2383,#2384,#2385));
#603=EDGE_LOOP('',(#2386,#2387,#2388,#2389));
#604=EDGE_LOOP('',(#2390,#2391,#2392,#2393));
#605=EDGE_LOOP('',(#2394,#2395,#2396,#2397));
#606=EDGE_LOOP('',(#2398,#2399,#2400,#2401,#2402,#2403,#2404,#2405));
#607=EDGE_LOOP('',(#2406));
#608=EDGE_LOOP('',(#2407,#2408,#2409,#2410));
#609=EDGE_LOOP('',(#2411,#2412,#2413,#2414));
#610=EDGE_LOOP('',(#2415));
#611=EDGE_LOOP('',(#2416));
#612=EDGE_LOOP('',(#2417,#2418,#2419,#2420));
#613=EDGE_LOOP('',(#2421));
#614=EDGE_LOOP('',(#2422));
#615=EDGE_LOOP('',(#2423));
#616=EDGE_LOOP('',(#2424));
#617=EDGE_LOOP('',(#2425,#2426,#2427,#2428));
#618=EDGE_LOOP('',(#2429,#2430,#2431,#2432));
#619=EDGE_LOOP('',(#2433,#2434,#2435,#2436,#2437,#2438,#2439,#2440));
#620=EDGE_LOOP('',(#2441,#2442,#2443,#2444));
#621=EDGE_LOOP('',(#2445,#2446,#2447,#2448));
#622=EDGE_LOOP('',(#2449,#2450,#2451,#2452));
#623=EDGE_LOOP('',(#2453,#2454,#2455,#2456));
#624=EDGE_LOOP('',(#2457,#2458,#2459,#2460));
#625=EDGE_LOOP('',(#2461,#2462,#2463,#2464));
#626=EDGE_LOOP('',(#2465,#2466,#2467,#2468,#2469,#2470,#2471,#2472));
#627=LINE('',#3890,#881);
#628=LINE('',#3897,#882);
#629=LINE('',#3904,#883);
#630=LINE('',#3911,#884);
#631=LINE('',#3918,#885);
#632=LINE('',#3925,#886);
#633=LINE('',#3931,#887);
#634=LINE('',#3933,#888);
#635=LINE('',#3935,#889);
#636=LINE('',#3936,#890);
#637=LINE('',#3939,#891);
#638=LINE('',#3941,#892);
#639=LINE('',#3942,#893);
#640=LINE('',#3945,#894);
#641=LINE('',#3947,#895);
#642=LINE('',#3948,#896);
#643=LINE('',#3950,#897);
#644=LINE('',#3951,#898);
#645=LINE('',#3959,#899);
#646=LINE('',#3966,#900);
#647=LINE('',#3973,#901);
#648=LINE('',#3980,#902);
#649=LINE('',#3987,#903);
#650=LINE('',#3994,#904);
#651=LINE('',#4000,#905);
#652=LINE('',#4002,#906);
#653=LINE('',#4004,#907);
#654=LINE('',#4005,#908);
#655=LINE('',#4008,#909);
#656=LINE('',#4010,#910);
#657=LINE('',#4011,#911);
#658=LINE('',#4014,#912);
#659=LINE('',#4016,#913);
#660=LINE('',#4017,#914);
#661=LINE('',#4019,#915);
#662=LINE('',#4020,#916);
#663=LINE('',#4028,#917);
#664=LINE('',#4036,#918);
#665=LINE('',#4040,#919);
#666=LINE('',#4044,#920);
#667=LINE('',#4047,#921);
#668=LINE('',#4050,#922);
#669=LINE('',#4053,#923);
#670=LINE('',#4057,#924);
#671=LINE('',#4061,#925);
#672=LINE('',#4065,#926);
#673=LINE('',#4067,#927);
#674=LINE('',#4070,#928);
#675=LINE('',#4071,#929);
#676=LINE('',#4074,#930);
#677=LINE('',#4076,#931);
#678=LINE('',#4079,#932);
#679=LINE('',#4080,#933);
#680=LINE('',#4083,#934);
#681=LINE('',#4085,#935);
#682=LINE('',#4086,#936);
#683=LINE('',#4089,#937);
#684=LINE('',#4090,#938);
#685=LINE('',#4093,#939);
#686=LINE('',#4094,#940);
#687=LINE('',#4097,#941);
#688=LINE('',#4098,#942);
#689=LINE('',#4102,#943);
#690=LINE('',#4104,#944);
#691=LINE('',#4105,#945);
#692=LINE('',#4107,#946);
#693=LINE('',#4110,#947);
#694=LINE('',#4111,#948);
#695=LINE('',#4113,#949);
#696=LINE('',#4119,#950);
#697=LINE('',#4123,#951);
#698=LINE('',#4127,#952);
#699=LINE('',#4130,#953);
#700=LINE('',#4134,#954);
#701=LINE('',#4138,#955);
#702=LINE('',#4141,#956);
#703=LINE('',#4142,#957);
#704=LINE('',#4145,#958);
#705=LINE('',#4147,#959);
#706=LINE('',#4151,#960);
#707=LINE('',#4153,#961);
#708=LINE('',#4157,#962);
#709=LINE('',#4159,#963);
#710=LINE('',#4162,#964);
#711=LINE('',#4163,#965);
#712=LINE('',#4166,#966);
#713=LINE('',#4168,#967);
#714=LINE('',#4169,#968);
#715=LINE('',#4172,#969);
#716=LINE('',#4174,#970);
#717=LINE('',#4176,#971);
#718=LINE('',#4177,#972);
#719=LINE('',#4180,#973);
#720=LINE('',#4181,#974);
#721=LINE('',#4184,#975);
#722=LINE('',#4185,#976);
#723=LINE('',#4189,#977);
#724=LINE('',#4191,#978);
#725=LINE('',#4192,#979);
#726=LINE('',#4195,#980);
#727=LINE('',#4196,#981);
#728=LINE('',#4198,#982);
#729=LINE('',#4201,#983);
#730=LINE('',#4202,#984);
#731=LINE('',#4205,#985);
#732=LINE('',#4206,#986);
#733=LINE('',#4208,#987);
#734=LINE('',#4215,#988);
#735=LINE('',#4221,#989);
#736=LINE('',#4228,#990);
#737=LINE('',#4236,#991);
#738=LINE('',#4238,#992);
#739=LINE('',#4240,#993);
#740=LINE('',#4241,#994);
#741=LINE('',#4244,#995);
#742=LINE('',#4246,#996);
#743=LINE('',#4247,#997);
#744=LINE('',#4250,#998);
#745=LINE('',#4252,#999);
#746=LINE('',#4253,#1000);
#747=LINE('',#4256,#1001);
#748=LINE('',#4258,#1002);
#749=LINE('',#4259,#1003);
#750=LINE('',#4262,#1004);
#751=LINE('',#4264,#1005);
#752=LINE('',#4265,#1006);
#753=LINE('',#4268,#1007);
#754=LINE('',#4270,#1008);
#755=LINE('',#4271,#1009);
#756=LINE('',#4274,#1010);
#757=LINE('',#4276,#1011);
#758=LINE('',#4277,#1012);
#759=LINE('',#4280,#1013);
#760=LINE('',#4282,#1014);
#761=LINE('',#4283,#1015);
#762=LINE('',#4285,#1016);
#763=LINE('',#4286,#1017);
#764=LINE('',#4294,#1018);
#765=LINE('',#4388,#1019);
#766=LINE('',#4394,#1020);
#767=LINE('',#4400,#1021);
#768=LINE('',#4406,#1022);
#769=LINE('',#4500,#1023);
#770=LINE('',#4506,#1024);
#771=LINE('',#4512,#1025);
#772=LINE('',#4525,#1026);
#773=LINE('',#4526,#1027);
#774=LINE('',#4538,#1028);
#775=LINE('',#4539,#1029);
#776=LINE('',#4551,#1030);
#777=LINE('',#4552,#1031);
#778=LINE('',#4554,#1032);
#779=LINE('',#4555,#1033);
#780=LINE('',#4567,#1034);
#781=LINE('',#4568,#1035);
#782=LINE('',#4570,#1036);
#783=LINE('',#4571,#1037);
#784=LINE('',#4573,#1038);
#785=LINE('',#4574,#1039);
#786=LINE('',#4576,#1040);
#787=LINE('',#4577,#1041);
#788=LINE('',#4580,#1042);
#789=LINE('',#4582,#1043);
#790=LINE('',#4584,#1044);
#791=LINE('',#4586,#1045);
#792=LINE('',#4588,#1046);
#793=LINE('',#4590,#1047);
#794=LINE('',#4592,#1048);
#795=LINE('',#4594,#1049);
#796=LINE('',#4596,#1050);
#797=LINE('',#4598,#1051);
#798=LINE('',#4600,#1052);
#799=LINE('',#4602,#1053);
#800=LINE('',#4603,#1054);
#801=LINE('',#4607,#1055);
#802=LINE('',#4610,#1056);
#803=LINE('',#4611,#1057);
#804=LINE('',#4615,#1058);
#805=LINE('',#4620,#1059);
#806=LINE('',#4621,#1060);
#807=LINE('',#4622,#1061);
#808=LINE('',#4626,#1062);
#809=LINE('',#4627,#1063);
#810=LINE('',#4628,#1064);
#811=LINE('',#4630,#1065);
#812=LINE('',#4633,#1066);
#813=LINE('',#4634,#1067);
#814=LINE('',#4638,#1068);
#815=LINE('',#4639,#1069);
#816=LINE('',#4640,#1070);
#817=LINE('',#4642,#1071);
#818=LINE('',#4644,#1072);
#819=LINE('',#4645,#1073);
#820=LINE('',#4648,#1074);
#821=LINE('',#4649,#1075);
#822=LINE('',#4652,#1076);
#823=LINE('',#4653,#1077);
#824=LINE('',#4656,#1078);
#825=LINE('',#4657,#1079);
#826=LINE('',#4660,#1080);
#827=LINE('',#4661,#1081);
#828=LINE('',#4663,#1082);
#829=LINE('',#4671,#1083);
#830=LINE('',#4677,#1084);
#831=LINE('',#4679,#1085);
#832=LINE('',#4681,#1086);
#833=LINE('',#4682,#1087);
#834=LINE('',#4685,#1088);
#835=LINE('',#4687,#1089);
#836=LINE('',#4689,#1090);
#837=LINE('',#4691,#1091);
#838=LINE('',#4693,#1092);
#839=LINE('',#4695,#1093);
#840=LINE('',#4696,#1094);
#841=LINE('',#4699,#1095);
#842=LINE('',#4700,#1096);
#843=LINE('',#4703,#1097);
#844=LINE('',#4704,#1098);
#845=LINE('',#4708,#1099);
#846=LINE('',#4709,#1100);
#847=LINE('',#4710,#1101);
#848=LINE('',#4713,#1102);
#849=LINE('',#4714,#1103);
#850=LINE('',#4717,#1104);
#851=LINE('',#4718,#1105);
#852=LINE('',#4720,#1106);
#853=LINE('',#4722,#1107);
#854=LINE('',#4729,#1108);
#855=LINE('',#4735,#1109);
#856=LINE('',#4742,#1110);
#857=LINE('',#4750,#1111);
#858=LINE('',#4752,#1112);
#859=LINE('',#4754,#1113);
#860=LINE('',#4755,#1114);
#861=LINE('',#4758,#1115);
#862=LINE('',#4760,#1116);
#863=LINE('',#4761,#1117);
#864=LINE('',#4764,#1118);
#865=LINE('',#4766,#1119);
#866=LINE('',#4768,#1120);
#867=LINE('',#4770,#1121);
#868=LINE('',#4772,#1122);
#869=LINE('',#4773,#1123);
#870=LINE('',#4776,#1124);
#871=LINE('',#4777,#1125);
#872=LINE('',#4780,#1126);
#873=LINE('',#4781,#1127);
#874=LINE('',#4784,#1128);
#875=LINE('',#4786,#1129);
#876=LINE('',#4787,#1130);
#877=LINE('',#4789,#1131);
#878=LINE('',#4792,#1132);
#879=LINE('',#4793,#1133);
#880=LINE('',#4795,#1134);
#881=VECTOR('',#3098,4.);
#882=VECTOR('',#3107,4.);
#883=VECTOR('',#3116,4.);
#884=VECTOR('',#3125,4.);
#885=VECTOR('',#3134,4.);
#886=VECTOR('',#3143,4.);
#887=VECTOR('',#3150,10.);
#888=VECTOR('',#3151,10.);
#889=VECTOR('',#3152,10.);
#890=VECTOR('',#3153,10.);
#891=VECTOR('',#3156,10.);
#892=VECTOR('',#3157,10.);
#893=VECTOR('',#3158,10.);
#894=VECTOR('',#3161,10.);
#895=VECTOR('',#3162,10.);
#896=VECTOR('',#3163,10.);
#897=VECTOR('',#3166,10.);
#898=VECTOR('',#3167,10.);
#899=VECTOR('',#3178,4.);
#900=VECTOR('',#3187,4.);
#901=VECTOR('',#3196,4.);
#902=VECTOR('',#3205,4.);
#903=VECTOR('',#3214,4.);
#904=VECTOR('',#3223,4.);
#905=VECTOR('',#3230,10.);
#906=VECTOR('',#3231,10.);
#907=VECTOR('',#3232,10.);
#908=VECTOR('',#3233,10.);
#909=VECTOR('',#3236,10.);
#910=VECTOR('',#3237,10.);
#911=VECTOR('',#3238,10.);
#912=VECTOR('',#3241,10.);
#913=VECTOR('',#3242,10.);
#914=VECTOR('',#3243,10.);
#915=VECTOR('',#3246,10.);
#916=VECTOR('',#3247,10.);
#917=VECTOR('',#3258,6.);
#918=VECTOR('',#3269,10.);
#919=VECTOR('',#3272,10.);
#920=VECTOR('',#3277,10.);
#921=VECTOR('',#3280,10.);
#922=VECTOR('',#3283,10.);
#923=VECTOR('',#3286,10.);
#924=VECTOR('',#3289,10.);
#925=VECTOR('',#3292,10.);
#926=VECTOR('',#3297,10.);
#927=VECTOR('',#3298,10.);
#928=VECTOR('',#3303,10.);
#929=VECTOR('',#3304,10.);
#930=VECTOR('',#3307,10.);
#931=VECTOR('',#3308,10.);
#932=VECTOR('',#3313,10.);
#933=VECTOR('',#3314,10.);
#934=VECTOR('',#3317,10.);
#935=VECTOR('',#3318,10.);
#936=VECTOR('',#3319,10.);
#937=VECTOR('',#3322,10.);
#938=VECTOR('',#3323,10.);
#939=VECTOR('',#3326,10.);
#940=VECTOR('',#3327,10.);
#941=VECTOR('',#3330,10.);
#942=VECTOR('',#3331,10.);
#943=VECTOR('',#3336,10.);
#944=VECTOR('',#3337,10.);
#945=VECTOR('',#3338,10.);
#946=VECTOR('',#3341,10.);
#947=VECTOR('',#3344,10.);
#948=VECTOR('',#3345,10.);
#949=VECTOR('',#3348,10.);
#950=VECTOR('',#3355,10.);
#951=VECTOR('',#3358,10.);
#952=VECTOR('',#3363,10.);
#953=VECTOR('',#3366,10.);
#954=VECTOR('',#3369,10.);
#955=VECTOR('',#3372,10.);
#956=VECTOR('',#3377,10.);
#957=VECTOR('',#3378,10.);
#958=VECTOR('',#3381,10.);
#959=VECTOR('',#3382,10.);
#960=VECTOR('',#3387,10.);
#961=VECTOR('',#3388,10.);
#962=VECTOR('',#3393,10.);
#963=VECTOR('',#3394,10.);
#964=VECTOR('',#3399,10.);
#965=VECTOR('',#3400,10.);
#966=VECTOR('',#3403,10.);
#967=VECTOR('',#3404,10.);
#968=VECTOR('',#3405,10.);
#969=VECTOR('',#3408,10.);
#970=VECTOR('',#3409,10.);
#971=VECTOR('',#3410,10.);
#972=VECTOR('',#3411,10.);
#973=VECTOR('',#3414,10.);
#974=VECTOR('',#3415,10.);
#975=VECTOR('',#3418,10.);
#976=VECTOR('',#3419,10.);
#977=VECTOR('',#3424,10.);
#978=VECTOR('',#3425,10.);
#979=VECTOR('',#3426,10.);
#980=VECTOR('',#3429,10.);
#981=VECTOR('',#3430,10.);
#982=VECTOR('',#3433,10.);
#983=VECTOR('',#3436,10.);
#984=VECTOR('',#3437,10.);
#985=VECTOR('',#3440,10.);
#986=VECTOR('',#3441,10.);
#987=VECTOR('',#3444,10.);
#988=VECTOR('',#3453,7.);
#989=VECTOR('',#3460,6.);
#990=VECTOR('',#3469,11.);
#991=VECTOR('',#3480,10.);
#992=VECTOR('',#3481,10.);
#993=VECTOR('',#3482,10.);
#994=VECTOR('',#3483,10.);
#995=VECTOR('',#3486,10.);
#996=VECTOR('',#3487,10.);
#997=VECTOR('',#3488,10.);
#998=VECTOR('',#3491,10.);
#999=VECTOR('',#3492,10.);
#1000=VECTOR('',#3493,10.);
#1001=VECTOR('',#3496,10.);
#1002=VECTOR('',#3497,10.);
#1003=VECTOR('',#3498,10.);
#1004=VECTOR('',#3501,10.);
#1005=VECTOR('',#3502,10.);
#1006=VECTOR('',#3503,10.);
#1007=VECTOR('',#3506,10.);
#1008=VECTOR('',#3507,10.);
#1009=VECTOR('',#3508,10.);
#1010=VECTOR('',#3511,10.);
#1011=VECTOR('',#3512,10.);
#1012=VECTOR('',#3513,10.);
#1013=VECTOR('',#3516,10.);
#1014=VECTOR('',#3517,10.);
#1015=VECTOR('',#3518,10.);
#1016=VECTOR('',#3521,10.);
#1017=VECTOR('',#3522,10.);
#1018=VECTOR('',#3533,5.);
#1019=VECTOR('',#3536,5.);
#1020=VECTOR('',#3543,5.);
#1021=VECTOR('',#3550,5.);
#1022=VECTOR('',#3557,5.);
#1023=VECTOR('',#3560,5.);
#1024=VECTOR('',#3567,5.);
#1025=VECTOR('',#3574,5.);
#1026=VECTOR('',#3589,10.);
#1027=VECTOR('',#3590,10.);
#1028=VECTOR('',#3603,10.);
#1029=VECTOR('',#3604,10.);
#1030=VECTOR('',#3617,10.);
#1031=VECTOR('',#3618,10.);
#1032=VECTOR('',#3621,10.);
#1033=VECTOR('',#3622,10.);
#1034=VECTOR('',#3635,10.);
#1035=VECTOR('',#3636,10.);
#1036=VECTOR('',#3639,10.);
#1037=VECTOR('',#3640,10.);
#1038=VECTOR('',#3643,10.);
#1039=VECTOR('',#3644,10.);
#1040=VECTOR('',#3647,10.);
#1041=VECTOR('',#3648,10.);
#1042=VECTOR('',#3651,10.);
#1043=VECTOR('',#3652,10.);
#1044=VECTOR('',#3653,10.);
#1045=VECTOR('',#3654,10.);
#1046=VECTOR('',#3655,10.);
#1047=VECTOR('',#3656,10.);
#1048=VECTOR('',#3657,10.);
#1049=VECTOR('',#3658,10.);
#1050=VECTOR('',#3659,10.);
#1051=VECTOR('',#3660,10.);
#1052=VECTOR('',#3661,10.);
#1053=VECTOR('',#3662,10.);
#1054=VECTOR('',#3663,10.);
#1055=VECTOR('',#3668,10.);
#1056=VECTOR('',#3671,10.);
#1057=VECTOR('',#3672,10.);
#1058=VECTOR('',#3677,6.);
#1059=VECTOR('',#3682,10.);
#1060=VECTOR('',#3683,10.);
#1061=VECTOR('',#3684,10.);
#1062=VECTOR('',#3687,10.);
#1063=VECTOR('',#3688,10.);
#1064=VECTOR('',#3689,10.);
#1065=VECTOR('',#3692,10.);
#1066=VECTOR('',#3695,10.);
#1067=VECTOR('',#3696,10.);
#1068=VECTOR('',#3699,10.);
#1069=VECTOR('',#3700,10.);
#1070=VECTOR('',#3701,10.);
#1071=VECTOR('',#3704,10.);
#1072=VECTOR('',#3707,10.);
#1073=VECTOR('',#3708,10.);
#1074=VECTOR('',#3711,10.);
#1075=VECTOR('',#3712,10.);
#1076=VECTOR('',#3715,10.);
#1077=VECTOR('',#3716,10.);
#1078=VECTOR('',#3719,10.);
#1079=VECTOR('',#3720,10.);
#1080=VECTOR('',#3723,10.);
#1081=VECTOR('',#3724,10.);
#1082=VECTOR('',#3727,10.);
#1083=VECTOR('',#3738,17.5);
#1084=VECTOR('',#3745,10.);
#1085=VECTOR('',#3746,10.);
#1086=VECTOR('',#3747,10.);
#1087=VECTOR('',#3748,10.);
#1088=VECTOR('',#3751,10.);
#1089=VECTOR('',#3752,10.);
#1090=VECTOR('',#3753,10.);
#1091=VECTOR('',#3754,10.);
#1092=VECTOR('',#3755,10.);
#1093=VECTOR('',#3756,10.);
#1094=VECTOR('',#3757,10.);
#1095=VECTOR('',#3760,10.);
#1096=VECTOR('',#3761,10.);
#1097=VECTOR('',#3764,10.);
#1098=VECTOR('',#3765,10.);
#1099=VECTOR('',#3768,10.);
#1100=VECTOR('',#3769,10.);
#1101=VECTOR('',#3770,10.);
#1102=VECTOR('',#3773,10.);
#1103=VECTOR('',#3774,10.);
#1104=VECTOR('',#3777,10.);
#1105=VECTOR('',#3778,10.);
#1106=VECTOR('',#3781,10.);
#1107=VECTOR('',#3784,10.);
#1108=VECTOR('',#3793,7.);
#1109=VECTOR('',#3800,6.);
#1110=VECTOR('',#3809,11.);
#1111=VECTOR('',#3820,10.);
#1112=VECTOR('',#3821,10.);
#1113=VECTOR('',#3822,10.);
#1114=VECTOR('',#3823,10.);
#1115=VECTOR('',#3826,10.);
#1116=VECTOR('',#3827,10.);
#1117=VECTOR('',#3828,10.);
#1118=VECTOR('',#3831,10.);
#1119=VECTOR('',#3832,10.);
#1120=VECTOR('',#3833,10.);
#1121=VECTOR('',#3834,10.);
#1122=VECTOR('',#3835,10.);
#1123=VECTOR('',#3836,10.);
#1124=VECTOR('',#3839,10.);
#1125=VECTOR('',#3840,10.);
#1126=VECTOR('',#3843,10.);
#1127=VECTOR('',#3844,10.);
#1128=VECTOR('',#3847,10.);
#1129=VECTOR('',#3848,10.);
#1130=VECTOR('',#3849,10.);
#1131=VECTOR('',#3852,10.);
#1132=VECTOR('',#3855,10.);
#1133=VECTOR('',#3856,10.);
#1134=VECTOR('',#3859,10.);
#1135=CIRCLE('',#2823,4.);
#1136=CIRCLE('',#2824,4.);
#1137=CIRCLE('',#2827,4.);
#1138=CIRCLE('',#2828,4.);
#1139=CIRCLE('',#2831,4.);
#1140=CIRCLE('',#2832,4.);
#1141=CIRCLE('',#2835,4.);
#1142=CIRCLE('',#2836,4.);
#1143=CIRCLE('',#2839,4.);
#1144=CIRCLE('',#2840,4.);
#1145=CIRCLE('',#2843,4.);
#1146=CIRCLE('',#2844,4.);
#1147=CIRCLE('',#2854,4.);
#1148=CIRCLE('',#2855,4.);
#1149=CIRCLE('',#2858,4.);
#1150=CIRCLE('',#2859,4.);
#1151=CIRCLE('',#2862,4.);
#1152=CIRCLE('',#2863,4.);
#1153=CIRCLE('',#2866,4.);
#1154=CIRCLE('',#2867,4.);
#1155=CIRCLE('',#2870,4.);
#1156=CIRCLE('',#2871,4.);
#1157=CIRCLE('',#2874,4.);
#1158=CIRCLE('',#2875,4.);
#1159=CIRCLE('',#2885,6.);
#1160=CIRCLE('',#2886,6.);
#1161=CIRCLE('',#2947,7.);
#1162=CIRCLE('',#2948,7.);
#1163=CIRCLE('',#2950,6.);
#1164=CIRCLE('',#2951,6.);
#1165=CIRCLE('',#2954,11.);
#1166=CIRCLE('',#2955,11.);
#1167=CIRCLE('',#2972,5.);
#1168=CIRCLE('',#2974,5.);
#1169=CIRCLE('',#2976,5.);
#1170=CIRCLE('',#2977,5.);
#1171=CIRCLE('',#2979,5.);
#1172=CIRCLE('',#2980,5.);
#1173=CIRCLE('',#2982,5.);
#1174=CIRCLE('',#2984,5.);
#1175=CIRCLE('',#2986,5.);
#1176=CIRCLE('',#2987,5.);
#1177=CIRCLE('',#2989,5.);
#1178=CIRCLE('',#2990,5.);
#1179=CIRCLE('',#2992,1.);
#1180=CIRCLE('',#2993,1.00000000000001);
#1181=CIRCLE('',#2994,1.);
#1182=CIRCLE('',#2996,1.);
#1183=CIRCLE('',#2998,0.999999999999996);
#1184=CIRCLE('',#2999,0.999999999999996);
#1185=CIRCLE('',#3000,1.);
#1186=CIRCLE('',#3002,1.);
#1187=CIRCLE('',#3004,0.999999999999996);
#1188=CIRCLE('',#3005,0.999999999999996);
#1189=CIRCLE('',#3006,1.);
#1190=CIRCLE('',#3008,1.);
#1191=CIRCLE('',#3011,0.999999999999996);
#1192=CIRCLE('',#3012,0.999999999999996);
#1193=CIRCLE('',#3013,1.);
#1194=CIRCLE('',#3015,1.);
#1195=CIRCLE('',#3020,6.);
#1196=CIRCLE('',#3025,6.);
#1197=CIRCLE('',#3042,17.5);
#1198=CIRCLE('',#3043,17.5);
#1199=CIRCLE('',#3057,7.);
#1200=CIRCLE('',#3058,7.);
#1201=CIRCLE('',#3060,6.);
#1202=CIRCLE('',#3061,6.);
#1203=CIRCLE('',#3064,11.);
#1204=CIRCLE('',#3065,11.);
#1205=VERTEX_POINT('',#3887);
#1206=VERTEX_POINT('',#3889);
#1207=VERTEX_POINT('',#3894);
#1208=VERTEX_POINT('',#3896);
#1209=VERTEX_POINT('',#3901);
#1210=VERTEX_POINT('',#3903);
#1211=VERTEX_POINT('',#3908);
#1212=VERTEX_POINT('',#3910);
#1213=VERTEX_POINT('',#3915);
#1214=VERTEX_POINT('',#3917);
#1215=VERTEX_POINT('',#3922);
#1216=VERTEX_POINT('',#3924);
#1217=VERTEX_POINT('',#3929);
#1218=VERTEX_POINT('',#3930);
#1219=VERTEX_POINT('',#3932);
#1220=VERTEX_POINT('',#3934);
#1221=VERTEX_POINT('',#3938);
#1222=VERTEX_POINT('',#3940);
#1223=VERTEX_POINT('',#3944);
#1224=VERTEX_POINT('',#3946);
#1225=VERTEX_POINT('',#3956);
#1226=VERTEX_POINT('',#3958);
#1227=VERTEX_POINT('',#3963);
#1228=VERTEX_POINT('',#3965);
#1229=VERTEX_POINT('',#3970);
#1230=VERTEX_POINT('',#3972);
#1231=VERTEX_POINT('',#3977);
#1232=VERTEX_POINT('',#3979);
#1233=VERTEX_POINT('',#3984);
#1234=VERTEX_POINT('',#3986);
#1235=VERTEX_POINT('',#3991);
#1236=VERTEX_POINT('',#3993);
#1237=VERTEX_POINT('',#3998);
#1238=VERTEX_POINT('',#3999);
#1239=VERTEX_POINT('',#4001);
#1240=VERTEX_POINT('',#4003);
#1241=VERTEX_POINT('',#4007);
#1242=VERTEX_POINT('',#4009);
#1243=VERTEX_POINT('',#4013);
#1244=VERTEX_POINT('',#4015);
#1245=VERTEX_POINT('',#4025);
#1246=VERTEX_POINT('',#4027);
#1247=VERTEX_POINT('',#4034);
#1248=VERTEX_POINT('',#4035);
#1249=VERTEX_POINT('',#4037);
#1250=VERTEX_POINT('',#4039);
#1251=VERTEX_POINT('',#4043);
#1252=VERTEX_POINT('',#4045);
#1253=VERTEX_POINT('',#4049);
#1254=VERTEX_POINT('',#4051);
#1255=VERTEX_POINT('',#4055);
#1256=VERTEX_POINT('',#4056);
#1257=VERTEX_POINT('',#4058);
#1258=VERTEX_POINT('',#4060);
#1259=VERTEX_POINT('',#4064);
#1260=VERTEX_POINT('',#4066);
#1261=VERTEX_POINT('',#4073);
#1262=VERTEX_POINT('',#4075);
#1263=VERTEX_POINT('',#4082);
#1264=VERTEX_POINT('',#4084);
#1265=VERTEX_POINT('',#4088);
#1266=VERTEX_POINT('',#4092);
#1267=VERTEX_POINT('',#4096);
#1268=VERTEX_POINT('',#4101);
#1269=VERTEX_POINT('',#4103);
#1270=VERTEX_POINT('',#4109);
#1271=VERTEX_POINT('',#4117);
#1272=VERTEX_POINT('',#4118);
#1273=VERTEX_POINT('',#4120);
#1274=VERTEX_POINT('',#4122);
#1275=VERTEX_POINT('',#4126);
#1276=VERTEX_POINT('',#4128);
#1277=VERTEX_POINT('',#4132);
#1278=VERTEX_POINT('',#4133);
#1279=VERTEX_POINT('',#4135);
#1280=VERTEX_POINT('',#4137);
#1281=VERTEX_POINT('',#4144);
#1282=VERTEX_POINT('',#4146);
#1283=VERTEX_POINT('',#4150);
#1284=VERTEX_POINT('',#4152);
#1285=VERTEX_POINT('',#4156);
#1286=VERTEX_POINT('',#4158);
#1287=VERTEX_POINT('',#4165);
#1288=VERTEX_POINT('',#4167);
#1289=VERTEX_POINT('',#4171);
#1290=VERTEX_POINT('',#4173);
#1291=VERTEX_POINT('',#4175);
#1292=VERTEX_POINT('',#4179);
#1293=VERTEX_POINT('',#4183);
#1294=VERTEX_POINT('',#4188);
#1295=VERTEX_POINT('',#4190);
#1296=VERTEX_POINT('',#4194);
#1297=VERTEX_POINT('',#4200);
#1298=VERTEX_POINT('',#4204);
#1299=VERTEX_POINT('',#4212);
#1300=VERTEX_POINT('',#4214);
#1301=VERTEX_POINT('',#4218);
#1302=VERTEX_POINT('',#4220);
#1303=VERTEX_POINT('',#4225);
#1304=VERTEX_POINT('',#4227);
#1305=VERTEX_POINT('',#4234);
#1306=VERTEX_POINT('',#4235);
#1307=VERTEX_POINT('',#4237);
#1308=VERTEX_POINT('',#4239);
#1309=VERTEX_POINT('',#4243);
#1310=VERTEX_POINT('',#4245);
#1311=VERTEX_POINT('',#4249);
#1312=VERTEX_POINT('',#4251);
#1313=VERTEX_POINT('',#4255);
#1314=VERTEX_POINT('',#4257);
#1315=VERTEX_POINT('',#4261);
#1316=VERTEX_POINT('',#4263);
#1317=VERTEX_POINT('',#4267);
#1318=VERTEX_POINT('',#4269);
#1319=VERTEX_POINT('',#4273);
#1320=VERTEX_POINT('',#4275);
#1321=VERTEX_POINT('',#4279);
#1322=VERTEX_POINT('',#4281);
#1323=VERTEX_POINT('',#4291);
#1324=VERTEX_POINT('',#4293);
#1325=VERTEX_POINT('',#4295);
#1326=VERTEX_POINT('',#4341);
#1327=VERTEX_POINT('',#4342);
#1328=VERTEX_POINT('',#4387);
#1329=VERTEX_POINT('',#4391);
#1330=VERTEX_POINT('',#4393);
#1331=VERTEX_POINT('',#4397);
#1332=VERTEX_POINT('',#4399);
#1333=VERTEX_POINT('',#4403);
#1334=VERTEX_POINT('',#4405);
#1335=VERTEX_POINT('',#4407);
#1336=VERTEX_POINT('',#4453);
#1337=VERTEX_POINT('',#4454);
#1338=VERTEX_POINT('',#4499);
#1339=VERTEX_POINT('',#4503);
#1340=VERTEX_POINT('',#4505);
#1341=VERTEX_POINT('',#4509);
#1342=VERTEX_POINT('',#4511);
#1343=VERTEX_POINT('',#4515);
#1344=VERTEX_POINT('',#4516);
#1345=VERTEX_POINT('',#4518);
#1346=VERTEX_POINT('',#4522);
#1347=VERTEX_POINT('',#4523);
#1348=VERTEX_POINT('',#4528);
#1349=VERTEX_POINT('',#4529);
#1350=VERTEX_POINT('',#4531);
#1351=VERTEX_POINT('',#4535);
#1352=VERTEX_POINT('',#4536);
#1353=VERTEX_POINT('',#4541);
#1354=VERTEX_POINT('',#4542);
#1355=VERTEX_POINT('',#4544);
#1356=VERTEX_POINT('',#4548);
#1357=VERTEX_POINT('',#4549);
#1358=VERTEX_POINT('',#4557);
#1359=VERTEX_POINT('',#4558);
#1360=VERTEX_POINT('',#4560);
#1361=VERTEX_POINT('',#4564);
#1362=VERTEX_POINT('',#4565);
#1363=VERTEX_POINT('',#4579);
#1364=VERTEX_POINT('',#4581);
#1365=VERTEX_POINT('',#4583);
#1366=VERTEX_POINT('',#4585);
#1367=VERTEX_POINT('',#4587);
#1368=VERTEX_POINT('',#4589);
#1369=VERTEX_POINT('',#4591);
#1370=VERTEX_POINT('',#4593);
#1371=VERTEX_POINT('',#4595);
#1372=VERTEX_POINT('',#4597);
#1373=VERTEX_POINT('',#4599);
#1374=VERTEX_POINT('',#4601);
#1375=VERTEX_POINT('',#4604);
#1376=VERTEX_POINT('',#4609);
#1377=VERTEX_POINT('',#4614);
#1378=VERTEX_POINT('',#4618);
#1379=VERTEX_POINT('',#4619);
#1380=VERTEX_POINT('',#4624);
#1381=VERTEX_POINT('',#4625);
#1382=VERTEX_POINT('',#4632);
#1383=VERTEX_POINT('',#4636);
#1384=VERTEX_POINT('',#4637);
#1385=VERTEX_POINT('',#4647);
#1386=VERTEX_POINT('',#4651);
#1387=VERTEX_POINT('',#4655);
#1388=VERTEX_POINT('',#4659);
#1389=VERTEX_POINT('',#4668);
#1390=VERTEX_POINT('',#4670);
#1391=VERTEX_POINT('',#4675);
#1392=VERTEX_POINT('',#4676);
#1393=VERTEX_POINT('',#4678);
#1394=VERTEX_POINT('',#4680);
#1395=VERTEX_POINT('',#4684);
#1396=VERTEX_POINT('',#4686);
#1397=VERTEX_POINT('',#4688);
#1398=VERTEX_POINT('',#4690);
#1399=VERTEX_POINT('',#4692);
#1400=VERTEX_POINT('',#4694);
#1401=VERTEX_POINT('',#4698);
#1402=VERTEX_POINT('',#4702);
#1403=VERTEX_POINT('',#4706);
#1404=VERTEX_POINT('',#4707);
#1405=VERTEX_POINT('',#4712);
#1406=VERTEX_POINT('',#4716);
#1407=VERTEX_POINT('',#4726);
#1408=VERTEX_POINT('',#4728);
#1409=VERTEX_POINT('',#4732);
#1410=VERTEX_POINT('',#4734);
#1411=VERTEX_POINT('',#4739);
#1412=VERTEX_POINT('',#4741);
#1413=VERTEX_POINT('',#4748);
#1414=VERTEX_POINT('',#4749);
#1415=VERTEX_POINT('',#4751);
#1416=VERTEX_POINT('',#4753);
#1417=VERTEX_POINT('',#4757);
#1418=VERTEX_POINT('',#4759);
#1419=VERTEX_POINT('',#4763);
#1420=VERTEX_POINT('',#4765);
#1421=VERTEX_POINT('',#4767);
#1422=VERTEX_POINT('',#4769);
#1423=VERTEX_POINT('',#4771);
#1424=VERTEX_POINT('',#4775);
#1425=VERTEX_POINT('',#4779);
#1426=VERTEX_POINT('',#4783);
#1427=VERTEX_POINT('',#4785);
#1428=VERTEX_POINT('',#4791);
#1429=EDGE_CURVE('',#1205,#1205,#1135,.T.);
#1430=EDGE_CURVE('',#1205,#1206,#627,.T.);
#1431=EDGE_CURVE('',#1206,#1206,#1136,.T.);
#1432=EDGE_CURVE('',#1207,#1207,#1137,.T.);
#1433=EDGE_CURVE('',#1207,#1208,#628,.T.);
#1434=EDGE_CURVE('',#1208,#1208,#1138,.T.);
#1435=EDGE_CURVE('',#1209,#1209,#1139,.T.);
#1436=EDGE_CURVE('',#1209,#1210,#629,.T.);
#1437=EDGE_CURVE('',#1210,#1210,#1140,.T.);
#1438=EDGE_CURVE('',#1211,#1211,#1141,.T.);
#1439=EDGE_CURVE('',#1211,#1212,#630,.T.);
#1440=EDGE_CURVE('',#1212,#1212,#1142,.T.);
#1441=EDGE_CURVE('',#1213,#1213,#1143,.T.);
#1442=EDGE_CURVE('',#1213,#1214,#631,.T.);
#1443=EDGE_CURVE('',#1214,#1214,#1144,.T.);
#1444=EDGE_CURVE('',#1215,#1215,#1145,.T.);
#1445=EDGE_CURVE('',#1215,#1216,#632,.T.);
#1446=EDGE_CURVE('',#1216,#1216,#1146,.T.);
#1447=EDGE_CURVE('',#1217,#1218,#633,.T.);
#1448=EDGE_CURVE('',#1218,#1219,#634,.T.);
#1449=EDGE_CURVE('',#1220,#1219,#635,.T.);
#1450=EDGE_CURVE('',#1217,#1220,#636,.T.);
#1451=EDGE_CURVE('',#1221,#1217,#637,.T.);
#1452=EDGE_CURVE('',#1222,#1220,#638,.T.);
#1453=EDGE_CURVE('',#1221,#1222,#639,.T.);
#1454=EDGE_CURVE('',#1223,#1221,#640,.T.);
#1455=EDGE_CURVE('',#1224,#1222,#641,.T.);
#1456=EDGE_CURVE('',#1223,#1224,#642,.T.);
#1457=EDGE_CURVE('',#1218,#1223,#643,.T.);
#1458=EDGE_CURVE('',#1219,#1224,#644,.T.);
#1459=EDGE_CURVE('',#1225,#1225,#1147,.T.);
#1460=EDGE_CURVE('',#1225,#1226,#645,.T.);
#1461=EDGE_CURVE('',#1226,#1226,#1148,.T.);
#1462=EDGE_CURVE('',#1227,#1227,#1149,.T.);
#1463=EDGE_CURVE('',#1227,#1228,#646,.T.);
#1464=EDGE_CURVE('',#1228,#1228,#1150,.T.);
#1465=EDGE_CURVE('',#1229,#1229,#1151,.T.);
#1466=EDGE_CURVE('',#1229,#1230,#647,.T.);
#1467=EDGE_CURVE('',#1230,#1230,#1152,.T.);
#1468=EDGE_CURVE('',#1231,#1231,#1153,.T.);
#1469=EDGE_CURVE('',#1231,#1232,#648,.T.);
#1470=EDGE_CURVE('',#1232,#1232,#1154,.T.);
#1471=EDGE_CURVE('',#1233,#1233,#1155,.T.);
#1472=EDGE_CURVE('',#1233,#1234,#649,.T.);
#1473=EDGE_CURVE('',#1234,#1234,#1156,.T.);
#1474=EDGE_CURVE('',#1235,#1235,#1157,.T.);
#1475=EDGE_CURVE('',#1235,#1236,#650,.T.);
#1476=EDGE_CURVE('',#1236,#1236,#1158,.T.);
#1477=EDGE_CURVE('',#1237,#1238,#651,.T.);
#1478=EDGE_CURVE('',#1237,#1239,#652,.T.);
#1479=EDGE_CURVE('',#1240,#1239,#653,.T.);
#1480=EDGE_CURVE('',#1238,#1240,#654,.T.);
#1481=EDGE_CURVE('',#1238,#1241,#655,.T.);
#1482=EDGE_CURVE('',#1242,#1240,#656,.T.);
#1483=EDGE_CURVE('',#1241,#1242,#657,.T.);
#1484=EDGE_CURVE('',#1241,#1243,#658,.T.);
#1485=EDGE_CURVE('',#1244,#1242,#659,.T.);
#1486=EDGE_CURVE('',#1243,#1244,#660,.T.);
#1487=EDGE_CURVE('',#1243,#1237,#661,.T.);
#1488=EDGE_CURVE('',#1239,#1244,#662,.T.);
#1489=EDGE_CURVE('',#1245,#1245,#1159,.T.);
#1490=EDGE_CURVE('',#1245,#1246,#663,.T.);
#1491=EDGE_CURVE('',#1246,#1246,#1160,.T.);
#1492=EDGE_CURVE('',#1247,#1248,#664,.T.);
#1493=EDGE_CURVE('',#1248,#1249,#67,.T.);
#1494=EDGE_CURVE('',#1249,#1250,#665,.T.);
#1495=EDGE_CURVE('',#1250,#1247,#68,.T.);
#1496=EDGE_CURVE('',#1248,#1251,#666,.T.);
#1497=EDGE_CURVE('',#1251,#1252,#69,.T.);
#1498=EDGE_CURVE('',#1252,#1249,#667,.T.);
#1499=EDGE_CURVE('',#1251,#1253,#668,.T.);
#1500=EDGE_CURVE('',#1253,#1254,#70,.T.);
#1501=EDGE_CURVE('',#1254,#1252,#669,.T.);
#1502=EDGE_CURVE('',#1255,#1256,#670,.T.);
#1503=EDGE_CURVE('',#1256,#1257,#71,.T.);
#1504=EDGE_CURVE('',#1257,#1258,#671,.T.);
#1505=EDGE_CURVE('',#1258,#1255,#72,.T.);
#1506=EDGE_CURVE('',#1259,#1257,#672,.T.);
#1507=EDGE_CURVE('',#1256,#1260,#673,.T.);
#1508=EDGE_CURVE('',#1260,#1259,#73,.T.);
#1509=EDGE_CURVE('',#1253,#1255,#674,.T.);
#1510=EDGE_CURVE('',#1258,#1254,#675,.T.);
#1511=EDGE_CURVE('',#1261,#1259,#676,.T.);
#1512=EDGE_CURVE('',#1260,#1262,#677,.T.);
#1513=EDGE_CURVE('',#1262,#1261,#74,.T.);
#1514=EDGE_CURVE('',#1250,#1261,#678,.T.);
#1515=EDGE_CURVE('',#1262,#1247,#679,.T.);
#1516=EDGE_CURVE('',#1252,#1263,#680,.T.);
#1517=EDGE_CURVE('',#1264,#1263,#681,.T.);
#1518=EDGE_CURVE('',#1264,#1249,#682,.T.);
#1519=EDGE_CURVE('',#1265,#1254,#683,.T.);
#1520=EDGE_CURVE('',#1263,#1265,#684,.T.);
#1521=EDGE_CURVE('',#1258,#1266,#685,.T.);
#1522=EDGE_CURVE('',#1265,#1266,#686,.T.);
#1523=EDGE_CURVE('',#1267,#1257,#687,.T.);
#1524=EDGE_CURVE('',#1266,#1267,#688,.T.);
#1525=EDGE_CURVE('',#1268,#1261,#689,.T.);
#1526=EDGE_CURVE('',#1269,#1268,#690,.T.);
#1527=EDGE_CURVE('',#1259,#1269,#691,.T.);
#1528=EDGE_CURVE('',#1267,#1269,#692,.T.);
#1529=EDGE_CURVE('',#1270,#1264,#693,.T.);
#1530=EDGE_CURVE('',#1250,#1270,#694,.T.);
#1531=EDGE_CURVE('',#1268,#1270,#695,.T.);
#1532=EDGE_CURVE('',#1271,#1272,#696,.T.);
#1533=EDGE_CURVE('',#1272,#1273,#75,.T.);
#1534=EDGE_CURVE('',#1273,#1274,#697,.T.);
#1535=EDGE_CURVE('',#1271,#1274,#76,.T.);
#1536=EDGE_CURVE('',#1272,#1275,#698,.T.);
#1537=EDGE_CURVE('',#1275,#1276,#77,.T.);
#1538=EDGE_CURVE('',#1276,#1273,#699,.T.);
#1539=EDGE_CURVE('',#1277,#1278,#700,.T.);
#1540=EDGE_CURVE('',#1278,#1279,#78,.T.);
#1541=EDGE_CURVE('',#1279,#1280,#701,.T.);
#1542=EDGE_CURVE('',#1280,#1277,#79,.T.);
#1543=EDGE_CURVE('',#1275,#1279,#702,.T.);
#1544=EDGE_CURVE('',#1278,#1276,#703,.T.);
#1545=EDGE_CURVE('',#1281,#1277,#704,.T.);
#1546=EDGE_CURVE('',#1280,#1282,#705,.T.);
#1547=EDGE_CURVE('',#1282,#1281,#80,.T.);
#1548=EDGE_CURVE('',#1283,#1281,#706,.T.);
#1549=EDGE_CURVE('',#1282,#1284,#707,.T.);
#1550=EDGE_CURVE('',#1284,#1283,#81,.T.);
#1551=EDGE_CURVE('',#1285,#1283,#708,.T.);
#1552=EDGE_CURVE('',#1284,#1286,#709,.T.);
#1553=EDGE_CURVE('',#1286,#1285,#82,.T.);
#1554=EDGE_CURVE('',#1274,#1285,#710,.T.);
#1555=EDGE_CURVE('',#1286,#1271,#711,.T.);
#1556=EDGE_CURVE('',#1273,#1287,#712,.T.);
#1557=EDGE_CURVE('',#1288,#1287,#713,.T.);
#1558=EDGE_CURVE('',#1274,#1288,#714,.T.);
#1559=EDGE_CURVE('',#1276,#1289,#715,.T.);
#1560=EDGE_CURVE('',#1289,#1290,#716,.T.);
#1561=EDGE_CURVE('',#1290,#1291,#717,.T.);
#1562=EDGE_CURVE('',#1287,#1291,#718,.T.);
#1563=EDGE_CURVE('',#1278,#1292,#719,.T.);
#1564=EDGE_CURVE('',#1292,#1289,#720,.T.);
#1565=EDGE_CURVE('',#1277,#1293,#721,.T.);
#1566=EDGE_CURVE('',#1293,#1292,#722,.T.);
#1567=EDGE_CURVE('',#1291,#1294,#723,.T.);
#1568=EDGE_CURVE('',#1290,#1295,#724,.T.);
#1569=EDGE_CURVE('',#1294,#1295,#725,.T.);
#1570=EDGE_CURVE('',#1296,#1293,#726,.T.);
#1571=EDGE_CURVE('',#1295,#1296,#727,.T.);
#1572=EDGE_CURVE('',#1281,#1296,#728,.T.);
#1573=EDGE_CURVE('',#1297,#1288,#729,.T.);
#1574=EDGE_CURVE('',#1285,#1297,#730,.T.);
#1575=EDGE_CURVE('',#1298,#1297,#731,.T.);
#1576=EDGE_CURVE('',#1283,#1298,#732,.T.);
#1577=EDGE_CURVE('',#1294,#1298,#733,.T.);
#1578=EDGE_CURVE('',#1299,#1299,#1161,.T.);
#1579=EDGE_CURVE('',#1299,#1300,#734,.T.);
#1580=EDGE_CURVE('',#1300,#1300,#1162,.T.);
#1581=EDGE_CURVE('',#1301,#1301,#1163,.T.);
#1582=EDGE_CURVE('',#1301,#1302,#735,.T.);
#1583=EDGE_CURVE('',#1302,#1302,#1164,.T.);
#1584=EDGE_CURVE('',#1303,#1303,#1165,.T.);
#1585=EDGE_CURVE('',#1303,#1304,#736,.T.);
#1586=EDGE_CURVE('',#1304,#1304,#1166,.T.);
#1587=EDGE_CURVE('',#1305,#1306,#737,.T.);
#1588=EDGE_CURVE('',#1305,#1307,#738,.T.);
#1589=EDGE_CURVE('',#1308,#1307,#739,.T.);
#1590=EDGE_CURVE('',#1306,#1308,#740,.T.);
#1591=EDGE_CURVE('',#1307,#1309,#741,.T.);
#1592=EDGE_CURVE('',#1309,#1310,#742,.T.);
#1593=EDGE_CURVE('',#1310,#1308,#743,.T.);
#1594=EDGE_CURVE('',#1306,#1311,#744,.T.);
#1595=EDGE_CURVE('',#1311,#1312,#745,.T.);
#1596=EDGE_CURVE('',#1305,#1312,#746,.T.);
#1597=EDGE_CURVE('',#1311,#1313,#747,.T.);
#1598=EDGE_CURVE('',#1314,#1313,#748,.T.);
#1599=EDGE_CURVE('',#1312,#1314,#749,.T.);
#1600=EDGE_CURVE('',#1313,#1315,#750,.T.);
#1601=EDGE_CURVE('',#1315,#1316,#751,.T.);
#1602=EDGE_CURVE('',#1316,#1314,#752,.T.);
#1603=EDGE_CURVE('',#1317,#1310,#753,.T.);
#1604=EDGE_CURVE('',#1318,#1309,#754,.T.);
#1605=EDGE_CURVE('',#1317,#1318,#755,.T.);
#1606=EDGE_CURVE('',#1319,#1317,#756,.T.);
#1607=EDGE_CURVE('',#1320,#1318,#757,.T.);
#1608=EDGE_CURVE('',#1319,#1320,#758,.T.);
#1609=EDGE_CURVE('',#1321,#1319,#759,.T.);
#1610=EDGE_CURVE('',#1322,#1320,#760,.T.);
#1611=EDGE_CURVE('',#1321,#1322,#761,.T.);
#1612=EDGE_CURVE('',#1315,#1321,#762,.T.);
#1613=EDGE_CURVE('',#1322,#1316,#763,.T.);
#1614=EDGE_CURVE('',#1323,#1323,#1167,.T.);
#1615=EDGE_CURVE('',#1323,#1324,#764,.T.);
#1616=EDGE_CURVE('',#1325,#1324,#59,.T.);
#1617=EDGE_CURVE('',#1324,#1325,#60,.T.);
#1618=EDGE_CURVE('',#1326,#1327,#61,.T.);
#1619=EDGE_CURVE('',#1327,#1326,#62,.T.);
#1620=EDGE_CURVE('',#1327,#1328,#765,.T.);
#1621=EDGE_CURVE('',#1328,#1328,#1168,.T.);
#1622=EDGE_CURVE('',#1329,#1329,#1169,.T.);
#1623=EDGE_CURVE('',#1329,#1330,#766,.T.);
#1624=EDGE_CURVE('',#1330,#1330,#1170,.T.);
#1625=EDGE_CURVE('',#1331,#1331,#1171,.T.);
#1626=EDGE_CURVE('',#1331,#1332,#767,.T.);
#1627=EDGE_CURVE('',#1332,#1332,#1172,.T.);
#1628=EDGE_CURVE('',#1333,#1333,#1173,.T.);
#1629=EDGE_CURVE('',#1333,#1334,#768,.T.);
#1630=EDGE_CURVE('',#1335,#1334,#63,.T.);
#1631=EDGE_CURVE('',#1334,#1335,#64,.T.);
#1632=EDGE_CURVE('',#1336,#1337,#65,.T.);
#1633=EDGE_CURVE('',#1337,#1336,#66,.T.);
#1634=EDGE_CURVE('',#1337,#1338,#769,.T.);
#1635=EDGE_CURVE('',#1338,#1338,#1174,.T.);
#1636=EDGE_CURVE('',#1339,#1339,#1175,.T.);
#1637=EDGE_CURVE('',#1339,#1340,#770,.T.);
#1638=EDGE_CURVE('',#1340,#1340,#1176,.T.);
#1639=EDGE_CURVE('',#1341,#1341,#1177,.T.);
#1640=EDGE_CURVE('',#1341,#1342,#771,.T.);
#1641=EDGE_CURVE('',#1342,#1342,#1178,.T.);
#1642=EDGE_CURVE('',#1343,#1344,#1179,.F.);
#1643=EDGE_CURVE('',#1345,#1343,#1180,.F.);
#1644=EDGE_CURVE('',#1344,#1345,#1181,.F.);
#1645=EDGE_CURVE('',#1346,#1347,#1182,.T.);
#1646=EDGE_CURVE('',#1347,#1345,#772,.T.);
#1647=EDGE_CURVE('',#1343,#1346,#773,.T.);
#1648=EDGE_CURVE('',#1348,#1349,#1183,.F.);
#1649=EDGE_CURVE('',#1350,#1348,#1184,.F.);
#1650=EDGE_CURVE('',#1349,#1350,#1185,.F.);
#1651=EDGE_CURVE('',#1351,#1352,#1186,.T.);
#1652=EDGE_CURVE('',#1352,#1350,#774,.T.);
#1653=EDGE_CURVE('',#1348,#1351,#775,.T.);
#1654=EDGE_CURVE('',#1353,#1354,#1187,.F.);
#1655=EDGE_CURVE('',#1355,#1353,#1188,.F.);
#1656=EDGE_CURVE('',#1354,#1355,#1189,.F.);
#1657=EDGE_CURVE('',#1356,#1357,#1190,.T.);
#1658=EDGE_CURVE('',#1357,#1355,#776,.T.);
#1659=EDGE_CURVE('',#1353,#1356,#777,.T.);
#1660=EDGE_CURVE('',#1344,#1354,#778,.T.);
#1661=EDGE_CURVE('',#1355,#1343,#779,.T.);
#1662=EDGE_CURVE('',#1358,#1359,#1191,.F.);
#1663=EDGE_CURVE('',#1360,#1358,#1192,.F.);
#1664=EDGE_CURVE('',#1359,#1360,#1193,.F.);
#1665=EDGE_CURVE('',#1361,#1362,#1194,.T.);
#1666=EDGE_CURVE('',#1362,#1360,#780,.T.);
#1667=EDGE_CURVE('',#1358,#1361,#781,.T.);
#1668=EDGE_CURVE('',#1354,#1359,#782,.T.);
#1669=EDGE_CURVE('',#1360,#1353,#783,.T.);
#1670=EDGE_CURVE('',#1359,#1349,#784,.T.);
#1671=EDGE_CURVE('',#1350,#1358,#785,.T.);
#1672=EDGE_CURVE('',#1349,#1344,#786,.T.);
#1673=EDGE_CURVE('',#1345,#1348,#787,.T.);
#1674=EDGE_CURVE('',#1357,#1363,#788,.T.);
#1675=EDGE_CURVE('',#1363,#1364,#789,.T.);
#1676=EDGE_CURVE('',#1364,#1365,#790,.T.);
#1677=EDGE_CURVE('',#1365,#1366,#791,.T.);
#1678=EDGE_CURVE('',#1366,#1367,#792,.T.);
#1679=EDGE_CURVE('',#1367,#1368,#793,.T.);
#1680=EDGE_CURVE('',#1369,#1368,#794,.T.);
#1681=EDGE_CURVE('',#1369,#1370,#795,.T.);
#1682=EDGE_CURVE('',#1370,#1371,#796,.T.);
#1683=EDGE_CURVE('',#1371,#1372,#797,.T.);
#1684=EDGE_CURVE('',#1372,#1373,#798,.T.);
#1685=EDGE_CURVE('',#1373,#1374,#799,.T.);
#1686=EDGE_CURVE('',#1374,#1346,#800,.T.);
#1687=EDGE_CURVE('',#1375,#1375,#1195,.T.);
#1688=EDGE_CURVE('',#1362,#1356,#801,.T.);
#1689=EDGE_CURVE('',#1376,#1361,#802,.T.);
#1690=EDGE_CURVE('',#1376,#1363,#803,.T.);
#1691=EDGE_CURVE('',#1375,#1377,#804,.T.);
#1692=EDGE_CURVE('',#1377,#1377,#1196,.T.);
#1693=EDGE_CURVE('',#1378,#1379,#805,.T.);
#1694=EDGE_CURVE('',#1378,#1372,#806,.T.);
#1695=EDGE_CURVE('',#1379,#1371,#807,.T.);
#1696=EDGE_CURVE('',#1380,#1381,#808,.T.);
#1697=EDGE_CURVE('',#1374,#1380,#809,.T.);
#1698=EDGE_CURVE('',#1373,#1381,#810,.T.);
#1699=EDGE_CURVE('',#1381,#1378,#811,.T.);
#1700=EDGE_CURVE('',#1382,#1376,#812,.T.);
#1701=EDGE_CURVE('',#1382,#1364,#813,.T.);
#1702=EDGE_CURVE('',#1383,#1384,#814,.T.);
#1703=EDGE_CURVE('',#1366,#1383,#815,.T.);
#1704=EDGE_CURVE('',#1365,#1384,#816,.T.);
#1705=EDGE_CURVE('',#1384,#1382,#817,.T.);
#1706=EDGE_CURVE('',#1352,#1380,#818,.T.);
#1707=EDGE_CURVE('',#1347,#1351,#819,.T.);
#1708=EDGE_CURVE('',#1385,#1383,#820,.T.);
#1709=EDGE_CURVE('',#1367,#1385,#821,.T.);
#1710=EDGE_CURVE('',#1386,#1370,#822,.T.);
#1711=EDGE_CURVE('',#1379,#1386,#823,.T.);
#1712=EDGE_CURVE('',#1386,#1387,#824,.T.);
#1713=EDGE_CURVE('',#1387,#1369,#825,.T.);
#1714=EDGE_CURVE('',#1388,#1385,#826,.T.);
#1715=EDGE_CURVE('',#1368,#1388,#827,.T.);
#1716=EDGE_CURVE('',#1388,#1387,#828,.T.);
#1717=EDGE_CURVE('',#1389,#1389,#1197,.T.);
#1718=EDGE_CURVE('',#1389,#1390,#829,.T.);
#1719=EDGE_CURVE('',#1390,#1390,#1198,.T.);
#1720=EDGE_CURVE('',#1391,#1392,#830,.T.);
#1721=EDGE_CURVE('',#1392,#1393,#831,.T.);
#1722=EDGE_CURVE('',#1393,#1394,#832,.T.);
#1723=EDGE_CURVE('',#1394,#1391,#833,.T.);
#1724=EDGE_CURVE('',#1393,#1395,#834,.T.);
#1725=EDGE_CURVE('',#1396,#1395,#835,.T.);
#1726=EDGE_CURVE('',#1396,#1397,#836,.T.);
#1727=EDGE_CURVE('',#1398,#1397,#837,.T.);
#1728=EDGE_CURVE('',#1398,#1399,#838,.T.);
#1729=EDGE_CURVE('',#1400,#1399,#839,.T.);
#1730=EDGE_CURVE('',#1400,#1394,#840,.T.);
#1731=EDGE_CURVE('',#1401,#1392,#841,.T.);
#1732=EDGE_CURVE('',#1395,#1401,#842,.T.);
#1733=EDGE_CURVE('',#1401,#1402,#843,.T.);
#1734=EDGE_CURVE('',#1402,#1396,#844,.T.);
#1735=EDGE_CURVE('',#1403,#1404,#845,.T.);
#1736=EDGE_CURVE('',#1404,#1400,#846,.T.);
#1737=EDGE_CURVE('',#1399,#1403,#847,.T.);
#1738=EDGE_CURVE('',#1405,#1398,#848,.T.);
#1739=EDGE_CURVE('',#1403,#1405,#849,.T.);
#1740=EDGE_CURVE('',#1406,#1405,#850,.T.);
#1741=EDGE_CURVE('',#1397,#1406,#851,.T.);
#1742=EDGE_CURVE('',#1406,#1402,#852,.T.);
#1743=EDGE_CURVE('',#1391,#1404,#853,.T.);
#1744=EDGE_CURVE('',#1407,#1407,#1199,.T.);
#1745=EDGE_CURVE('',#1407,#1408,#854,.T.);
#1746=EDGE_CURVE('',#1408,#1408,#1200,.T.);
#1747=EDGE_CURVE('',#1409,#1409,#1201,.T.);
#1748=EDGE_CURVE('',#1409,#1410,#855,.T.);
#1749=EDGE_CURVE('',#1410,#1410,#1202,.T.);
#1750=EDGE_CURVE('',#1411,#1411,#1203,.T.);
#1751=EDGE_CURVE('',#1411,#1412,#856,.T.);
#1752=EDGE_CURVE('',#1412,#1412,#1204,.T.);
#1753=EDGE_CURVE('',#1413,#1414,#857,.T.);
#1754=EDGE_CURVE('',#1414,#1415,#858,.T.);
#1755=EDGE_CURVE('',#1415,#1416,#859,.T.);
#1756=EDGE_CURVE('',#1416,#1413,#860,.T.);
#1757=EDGE_CURVE('',#1417,#1414,#861,.T.);
#1758=EDGE_CURVE('',#1418,#1417,#862,.T.);
#1759=EDGE_CURVE('',#1418,#1415,#863,.T.);
#1760=EDGE_CURVE('',#1413,#1419,#864,.T.);
#1761=EDGE_CURVE('',#1420,#1419,#865,.T.);
#1762=EDGE_CURVE('',#1420,#1421,#866,.T.);
#1763=EDGE_CURVE('',#1422,#1421,#867,.T.);
#1764=EDGE_CURVE('',#1422,#1423,#868,.T.);
#1765=EDGE_CURVE('',#1417,#1423,#869,.T.);
#1766=EDGE_CURVE('',#1423,#1424,#870,.T.);
#1767=EDGE_CURVE('',#1424,#1418,#871,.T.);
#1768=EDGE_CURVE('',#1425,#1422,#872,.T.);
#1769=EDGE_CURVE('',#1425,#1424,#873,.T.);
#1770=EDGE_CURVE('',#1419,#1426,#874,.T.);
#1771=EDGE_CURVE('',#1426,#1427,#875,.T.);
#1772=EDGE_CURVE('',#1427,#1420,#876,.T.);
#1773=EDGE_CURVE('',#1416,#1426,#877,.T.);
#1774=EDGE_CURVE('',#1421,#1428,#878,.T.);
#1775=EDGE_CURVE('',#1428,#1425,#879,.T.);
#1776=EDGE_CURVE('',#1427,#1428,#880,.T.);
#1777=ORIENTED_EDGE('',*,*,#1429,.F.);
#1778=ORIENTED_EDGE('',*,*,#1430,.T.);
#1779=ORIENTED_EDGE('',*,*,#1431,.T.);
#1780=ORIENTED_EDGE('',*,*,#1430,.F.);
#1781=ORIENTED_EDGE('',*,*,#1431,.F.);
#1782=ORIENTED_EDGE('',*,*,#1432,.F.);
#1783=ORIENTED_EDGE('',*,*,#1433,.T.);
#1784=ORIENTED_EDGE('',*,*,#1434,.T.);
#1785=ORIENTED_EDGE('',*,*,#1433,.F.);
#1786=ORIENTED_EDGE('',*,*,#1434,.F.);
#1787=ORIENTED_EDGE('',*,*,#1435,.F.);
#1788=ORIENTED_EDGE('',*,*,#1436,.T.);
#1789=ORIENTED_EDGE('',*,*,#1437,.T.);
#1790=ORIENTED_EDGE('',*,*,#1436,.F.);
#1791=ORIENTED_EDGE('',*,*,#1437,.F.);
#1792=ORIENTED_EDGE('',*,*,#1438,.F.);
#1793=ORIENTED_EDGE('',*,*,#1439,.T.);
#1794=ORIENTED_EDGE('',*,*,#1440,.T.);
#1795=ORIENTED_EDGE('',*,*,#1439,.F.);
#1796=ORIENTED_EDGE('',*,*,#1440,.F.);
#1797=ORIENTED_EDGE('',*,*,#1441,.F.);
#1798=ORIENTED_EDGE('',*,*,#1442,.T.);
#1799=ORIENTED_EDGE('',*,*,#1443,.T.);
#1800=ORIENTED_EDGE('',*,*,#1442,.F.);
#1801=ORIENTED_EDGE('',*,*,#1443,.F.);
#1802=ORIENTED_EDGE('',*,*,#1444,.F.);
#1803=ORIENTED_EDGE('',*,*,#1445,.T.);
#1804=ORIENTED_EDGE('',*,*,#1446,.T.);
#1805=ORIENTED_EDGE('',*,*,#1445,.F.);
#1806=ORIENTED_EDGE('',*,*,#1446,.F.);
#1807=ORIENTED_EDGE('',*,*,#1447,.T.);
#1808=ORIENTED_EDGE('',*,*,#1448,.T.);
#1809=ORIENTED_EDGE('',*,*,#1449,.F.);
#1810=ORIENTED_EDGE('',*,*,#1450,.F.);
#1811=ORIENTED_EDGE('',*,*,#1451,.T.);
#1812=ORIENTED_EDGE('',*,*,#1450,.T.);
#1813=ORIENTED_EDGE('',*,*,#1452,.F.);
#1814=ORIENTED_EDGE('',*,*,#1453,.F.);
#1815=ORIENTED_EDGE('',*,*,#1454,.T.);
#1816=ORIENTED_EDGE('',*,*,#1453,.T.);
#1817=ORIENTED_EDGE('',*,*,#1455,.F.);
#1818=ORIENTED_EDGE('',*,*,#1456,.F.);
#1819=ORIENTED_EDGE('',*,*,#1457,.T.);
#1820=ORIENTED_EDGE('',*,*,#1456,.T.);
#1821=ORIENTED_EDGE('',*,*,#1458,.F.);
#1822=ORIENTED_EDGE('',*,*,#1448,.F.);
#1823=ORIENTED_EDGE('',*,*,#1458,.T.);
#1824=ORIENTED_EDGE('',*,*,#1455,.T.);
#1825=ORIENTED_EDGE('',*,*,#1452,.T.);
#1826=ORIENTED_EDGE('',*,*,#1449,.T.);
#1827=ORIENTED_EDGE('',*,*,#1444,.T.);
#1828=ORIENTED_EDGE('',*,*,#1441,.T.);
#1829=ORIENTED_EDGE('',*,*,#1438,.T.);
#1830=ORIENTED_EDGE('',*,*,#1435,.T.);
#1831=ORIENTED_EDGE('',*,*,#1432,.T.);
#1832=ORIENTED_EDGE('',*,*,#1429,.T.);
#1833=ORIENTED_EDGE('',*,*,#1457,.F.);
#1834=ORIENTED_EDGE('',*,*,#1447,.F.);
#1835=ORIENTED_EDGE('',*,*,#1451,.F.);
#1836=ORIENTED_EDGE('',*,*,#1454,.F.);
#1837=ORIENTED_EDGE('',*,*,#1459,.F.);
#1838=ORIENTED_EDGE('',*,*,#1460,.T.);
#1839=ORIENTED_EDGE('',*,*,#1461,.T.);
#1840=ORIENTED_EDGE('',*,*,#1460,.F.);
#1841=ORIENTED_EDGE('',*,*,#1461,.F.);
#1842=ORIENTED_EDGE('',*,*,#1462,.F.);
#1843=ORIENTED_EDGE('',*,*,#1463,.T.);
#1844=ORIENTED_EDGE('',*,*,#1464,.T.);
#1845=ORIENTED_EDGE('',*,*,#1463,.F.);
#1846=ORIENTED_EDGE('',*,*,#1464,.F.);
#1847=ORIENTED_EDGE('',*,*,#1465,.F.);
#1848=ORIENTED_EDGE('',*,*,#1466,.T.);
#1849=ORIENTED_EDGE('',*,*,#1467,.T.);
#1850=ORIENTED_EDGE('',*,*,#1466,.F.);
#1851=ORIENTED_EDGE('',*,*,#1467,.F.);
#1852=ORIENTED_EDGE('',*,*,#1468,.F.);
#1853=ORIENTED_EDGE('',*,*,#1469,.T.);
#1854=ORIENTED_EDGE('',*,*,#1470,.T.);
#1855=ORIENTED_EDGE('',*,*,#1469,.F.);
#1856=ORIENTED_EDGE('',*,*,#1470,.F.);
#1857=ORIENTED_EDGE('',*,*,#1471,.F.);
#1858=ORIENTED_EDGE('',*,*,#1472,.T.);
#1859=ORIENTED_EDGE('',*,*,#1473,.T.);
#1860=ORIENTED_EDGE('',*,*,#1472,.F.);
#1861=ORIENTED_EDGE('',*,*,#1473,.F.);
#1862=ORIENTED_EDGE('',*,*,#1474,.F.);
#1863=ORIENTED_EDGE('',*,*,#1475,.T.);
#1864=ORIENTED_EDGE('',*,*,#1476,.T.);
#1865=ORIENTED_EDGE('',*,*,#1475,.F.);
#1866=ORIENTED_EDGE('',*,*,#1476,.F.);
#1867=ORIENTED_EDGE('',*,*,#1477,.F.);
#1868=ORIENTED_EDGE('',*,*,#1478,.T.);
#1869=ORIENTED_EDGE('',*,*,#1479,.F.);
#1870=ORIENTED_EDGE('',*,*,#1480,.F.);
#1871=ORIENTED_EDGE('',*,*,#1481,.F.);
#1872=ORIENTED_EDGE('',*,*,#1480,.T.);
#1873=ORIENTED_EDGE('',*,*,#1482,.F.);
#1874=ORIENTED_EDGE('',*,*,#1483,.F.);
#1875=ORIENTED_EDGE('',*,*,#1484,.F.);
#1876=ORIENTED_EDGE('',*,*,#1483,.T.);
#1877=ORIENTED_EDGE('',*,*,#1485,.F.);
#1878=ORIENTED_EDGE('',*,*,#1486,.F.);
#1879=ORIENTED_EDGE('',*,*,#1487,.F.);
#1880=ORIENTED_EDGE('',*,*,#1486,.T.);
#1881=ORIENTED_EDGE('',*,*,#1488,.F.);
#1882=ORIENTED_EDGE('',*,*,#1478,.F.);
#1883=ORIENTED_EDGE('',*,*,#1488,.T.);
#1884=ORIENTED_EDGE('',*,*,#1485,.T.);
#1885=ORIENTED_EDGE('',*,*,#1482,.T.);
#1886=ORIENTED_EDGE('',*,*,#1479,.T.);
#1887=ORIENTED_EDGE('',*,*,#1474,.T.);
#1888=ORIENTED_EDGE('',*,*,#1471,.T.);
#1889=ORIENTED_EDGE('',*,*,#1468,.T.);
#1890=ORIENTED_EDGE('',*,*,#1465,.T.);
#1891=ORIENTED_EDGE('',*,*,#1462,.T.);
#1892=ORIENTED_EDGE('',*,*,#1459,.T.);
#1893=ORIENTED_EDGE('',*,*,#1487,.T.);
#1894=ORIENTED_EDGE('',*,*,#1477,.T.);
#1895=ORIENTED_EDGE('',*,*,#1481,.T.);
#1896=ORIENTED_EDGE('',*,*,#1484,.T.);
#1897=ORIENTED_EDGE('',*,*,#1489,.F.);
#1898=ORIENTED_EDGE('',*,*,#1490,.T.);
#1899=ORIENTED_EDGE('',*,*,#1491,.T.);
#1900=ORIENTED_EDGE('',*,*,#1490,.F.);
#1901=ORIENTED_EDGE('',*,*,#1489,.T.);
#1902=ORIENTED_EDGE('',*,*,#1491,.F.);
#1903=ORIENTED_EDGE('',*,*,#1492,.T.);
#1904=ORIENTED_EDGE('',*,*,#1493,.T.);
#1905=ORIENTED_EDGE('',*,*,#1494,.T.);
#1906=ORIENTED_EDGE('',*,*,#1495,.T.);
#1907=ORIENTED_EDGE('',*,*,#1496,.T.);
#1908=ORIENTED_EDGE('',*,*,#1497,.T.);
#1909=ORIENTED_EDGE('',*,*,#1498,.T.);
#1910=ORIENTED_EDGE('',*,*,#1493,.F.);
#1911=ORIENTED_EDGE('',*,*,#1499,.T.);
#1912=ORIENTED_EDGE('',*,*,#1500,.T.);
#1913=ORIENTED_EDGE('',*,*,#1501,.T.);
#1914=ORIENTED_EDGE('',*,*,#1497,.F.);
#1915=ORIENTED_EDGE('',*,*,#1502,.T.);
#1916=ORIENTED_EDGE('',*,*,#1503,.T.);
#1917=ORIENTED_EDGE('',*,*,#1504,.T.);
#1918=ORIENTED_EDGE('',*,*,#1505,.T.);
#1919=ORIENTED_EDGE('',*,*,#1506,.T.);
#1920=ORIENTED_EDGE('',*,*,#1503,.F.);
#1921=ORIENTED_EDGE('',*,*,#1507,.T.);
#1922=ORIENTED_EDGE('',*,*,#1508,.T.);
#1923=ORIENTED_EDGE('',*,*,#1509,.T.);
#1924=ORIENTED_EDGE('',*,*,#1505,.F.);
#1925=ORIENTED_EDGE('',*,*,#1510,.T.);
#1926=ORIENTED_EDGE('',*,*,#1500,.F.);
#1927=ORIENTED_EDGE('',*,*,#1511,.T.);
#1928=ORIENTED_EDGE('',*,*,#1508,.F.);
#1929=ORIENTED_EDGE('',*,*,#1512,.T.);
#1930=ORIENTED_EDGE('',*,*,#1513,.T.);
#1931=ORIENTED_EDGE('',*,*,#1514,.T.);
#1932=ORIENTED_EDGE('',*,*,#1513,.F.);
#1933=ORIENTED_EDGE('',*,*,#1515,.T.);
#1934=ORIENTED_EDGE('',*,*,#1495,.F.);
#1935=ORIENTED_EDGE('',*,*,#1498,.F.);
#1936=ORIENTED_EDGE('',*,*,#1516,.T.);
#1937=ORIENTED_EDGE('',*,*,#1517,.F.);
#1938=ORIENTED_EDGE('',*,*,#1518,.T.);
#1939=ORIENTED_EDGE('',*,*,#1501,.F.);
#1940=ORIENTED_EDGE('',*,*,#1519,.F.);
#1941=ORIENTED_EDGE('',*,*,#1520,.F.);
#1942=ORIENTED_EDGE('',*,*,#1516,.F.);
#1943=ORIENTED_EDGE('',*,*,#1510,.F.);
#1944=ORIENTED_EDGE('',*,*,#1521,.T.);
#1945=ORIENTED_EDGE('',*,*,#1522,.F.);
#1946=ORIENTED_EDGE('',*,*,#1519,.T.);
#1947=ORIENTED_EDGE('',*,*,#1504,.F.);
#1948=ORIENTED_EDGE('',*,*,#1523,.F.);
#1949=ORIENTED_EDGE('',*,*,#1524,.F.);
#1950=ORIENTED_EDGE('',*,*,#1521,.F.);
#1951=ORIENTED_EDGE('',*,*,#1502,.F.);
#1952=ORIENTED_EDGE('',*,*,#1509,.F.);
#1953=ORIENTED_EDGE('',*,*,#1499,.F.);
#1954=ORIENTED_EDGE('',*,*,#1496,.F.);
#1955=ORIENTED_EDGE('',*,*,#1492,.F.);
#1956=ORIENTED_EDGE('',*,*,#1515,.F.);
#1957=ORIENTED_EDGE('',*,*,#1512,.F.);
#1958=ORIENTED_EDGE('',*,*,#1507,.F.);
#1959=ORIENTED_EDGE('',*,*,#1511,.F.);
#1960=ORIENTED_EDGE('',*,*,#1525,.F.);
#1961=ORIENTED_EDGE('',*,*,#1526,.F.);
#1962=ORIENTED_EDGE('',*,*,#1527,.F.);
#1963=ORIENTED_EDGE('',*,*,#1506,.F.);
#1964=ORIENTED_EDGE('',*,*,#1527,.T.);
#1965=ORIENTED_EDGE('',*,*,#1528,.F.);
#1966=ORIENTED_EDGE('',*,*,#1523,.T.);
#1967=ORIENTED_EDGE('',*,*,#1494,.F.);
#1968=ORIENTED_EDGE('',*,*,#1518,.F.);
#1969=ORIENTED_EDGE('',*,*,#1529,.F.);
#1970=ORIENTED_EDGE('',*,*,#1530,.F.);
#1971=ORIENTED_EDGE('',*,*,#1514,.F.);
#1972=ORIENTED_EDGE('',*,*,#1530,.T.);
#1973=ORIENTED_EDGE('',*,*,#1531,.F.);
#1974=ORIENTED_EDGE('',*,*,#1525,.T.);
#1975=ORIENTED_EDGE('',*,*,#1524,.T.);
#1976=ORIENTED_EDGE('',*,*,#1528,.T.);
#1977=ORIENTED_EDGE('',*,*,#1526,.T.);
#1978=ORIENTED_EDGE('',*,*,#1531,.T.);
#1979=ORIENTED_EDGE('',*,*,#1529,.T.);
#1980=ORIENTED_EDGE('',*,*,#1517,.T.);
#1981=ORIENTED_EDGE('',*,*,#1520,.T.);
#1982=ORIENTED_EDGE('',*,*,#1522,.T.);
#1983=ORIENTED_EDGE('',*,*,#1532,.T.);
#1984=ORIENTED_EDGE('',*,*,#1533,.T.);
#1985=ORIENTED_EDGE('',*,*,#1534,.T.);
#1986=ORIENTED_EDGE('',*,*,#1535,.F.);
#1987=ORIENTED_EDGE('',*,*,#1536,.T.);
#1988=ORIENTED_EDGE('',*,*,#1537,.T.);
#1989=ORIENTED_EDGE('',*,*,#1538,.T.);
#1990=ORIENTED_EDGE('',*,*,#1533,.F.);
#1991=ORIENTED_EDGE('',*,*,#1539,.T.);
#1992=ORIENTED_EDGE('',*,*,#1540,.T.);
#1993=ORIENTED_EDGE('',*,*,#1541,.T.);
#1994=ORIENTED_EDGE('',*,*,#1542,.T.);
#1995=ORIENTED_EDGE('',*,*,#1543,.T.);
#1996=ORIENTED_EDGE('',*,*,#1540,.F.);
#1997=ORIENTED_EDGE('',*,*,#1544,.T.);
#1998=ORIENTED_EDGE('',*,*,#1537,.F.);
#1999=ORIENTED_EDGE('',*,*,#1545,.T.);
#2000=ORIENTED_EDGE('',*,*,#1542,.F.);
#2001=ORIENTED_EDGE('',*,*,#1546,.T.);
#2002=ORIENTED_EDGE('',*,*,#1547,.T.);
#2003=ORIENTED_EDGE('',*,*,#1548,.T.);
#2004=ORIENTED_EDGE('',*,*,#1547,.F.);
#2005=ORIENTED_EDGE('',*,*,#1549,.T.);
#2006=ORIENTED_EDGE('',*,*,#1550,.T.);
#2007=ORIENTED_EDGE('',*,*,#1551,.T.);
#2008=ORIENTED_EDGE('',*,*,#1550,.F.);
#2009=ORIENTED_EDGE('',*,*,#1552,.T.);
#2010=ORIENTED_EDGE('',*,*,#1553,.T.);
#2011=ORIENTED_EDGE('',*,*,#1554,.T.);
#2012=ORIENTED_EDGE('',*,*,#1553,.F.);
#2013=ORIENTED_EDGE('',*,*,#1555,.T.);
#2014=ORIENTED_EDGE('',*,*,#1535,.T.);
#2015=ORIENTED_EDGE('',*,*,#1534,.F.);
#2016=ORIENTED_EDGE('',*,*,#1556,.T.);
#2017=ORIENTED_EDGE('',*,*,#1557,.F.);
#2018=ORIENTED_EDGE('',*,*,#1558,.F.);
#2019=ORIENTED_EDGE('',*,*,#1538,.F.);
#2020=ORIENTED_EDGE('',*,*,#1559,.T.);
#2021=ORIENTED_EDGE('',*,*,#1560,.T.);
#2022=ORIENTED_EDGE('',*,*,#1561,.T.);
#2023=ORIENTED_EDGE('',*,*,#1562,.F.);
#2024=ORIENTED_EDGE('',*,*,#1556,.F.);
#2025=ORIENTED_EDGE('',*,*,#1544,.F.);
#2026=ORIENTED_EDGE('',*,*,#1563,.T.);
#2027=ORIENTED_EDGE('',*,*,#1564,.T.);
#2028=ORIENTED_EDGE('',*,*,#1559,.F.);
#2029=ORIENTED_EDGE('',*,*,#1539,.F.);
#2030=ORIENTED_EDGE('',*,*,#1565,.T.);
#2031=ORIENTED_EDGE('',*,*,#1566,.T.);
#2032=ORIENTED_EDGE('',*,*,#1563,.F.);
#2033=ORIENTED_EDGE('',*,*,#1541,.F.);
#2034=ORIENTED_EDGE('',*,*,#1543,.F.);
#2035=ORIENTED_EDGE('',*,*,#1536,.F.);
#2036=ORIENTED_EDGE('',*,*,#1532,.F.);
#2037=ORIENTED_EDGE('',*,*,#1555,.F.);
#2038=ORIENTED_EDGE('',*,*,#1552,.F.);
#2039=ORIENTED_EDGE('',*,*,#1549,.F.);
#2040=ORIENTED_EDGE('',*,*,#1546,.F.);
#2041=ORIENTED_EDGE('',*,*,#1567,.F.);
#2042=ORIENTED_EDGE('',*,*,#1561,.F.);
#2043=ORIENTED_EDGE('',*,*,#1568,.T.);
#2044=ORIENTED_EDGE('',*,*,#1569,.F.);
#2045=ORIENTED_EDGE('',*,*,#1564,.F.);
#2046=ORIENTED_EDGE('',*,*,#1566,.F.);
#2047=ORIENTED_EDGE('',*,*,#1570,.F.);
#2048=ORIENTED_EDGE('',*,*,#1571,.F.);
#2049=ORIENTED_EDGE('',*,*,#1568,.F.);
#2050=ORIENTED_EDGE('',*,*,#1560,.F.);
#2051=ORIENTED_EDGE('',*,*,#1545,.F.);
#2052=ORIENTED_EDGE('',*,*,#1572,.T.);
#2053=ORIENTED_EDGE('',*,*,#1570,.T.);
#2054=ORIENTED_EDGE('',*,*,#1565,.F.);
#2055=ORIENTED_EDGE('',*,*,#1554,.F.);
#2056=ORIENTED_EDGE('',*,*,#1558,.T.);
#2057=ORIENTED_EDGE('',*,*,#1573,.F.);
#2058=ORIENTED_EDGE('',*,*,#1574,.F.);
#2059=ORIENTED_EDGE('',*,*,#1551,.F.);
#2060=ORIENTED_EDGE('',*,*,#1574,.T.);
#2061=ORIENTED_EDGE('',*,*,#1575,.F.);
#2062=ORIENTED_EDGE('',*,*,#1576,.F.);
#2063=ORIENTED_EDGE('',*,*,#1548,.F.);
#2064=ORIENTED_EDGE('',*,*,#1576,.T.);
#2065=ORIENTED_EDGE('',*,*,#1577,.F.);
#2066=ORIENTED_EDGE('',*,*,#1569,.T.);
#2067=ORIENTED_EDGE('',*,*,#1571,.T.);
#2068=ORIENTED_EDGE('',*,*,#1572,.F.);
#2069=ORIENTED_EDGE('',*,*,#1567,.T.);
#2070=ORIENTED_EDGE('',*,*,#1577,.T.);
#2071=ORIENTED_EDGE('',*,*,#1575,.T.);
#2072=ORIENTED_EDGE('',*,*,#1573,.T.);
#2073=ORIENTED_EDGE('',*,*,#1557,.T.);
#2074=ORIENTED_EDGE('',*,*,#1562,.T.);
#2075=ORIENTED_EDGE('',*,*,#1578,.F.);
#2076=ORIENTED_EDGE('',*,*,#1579,.T.);
#2077=ORIENTED_EDGE('',*,*,#1580,.F.);
#2078=ORIENTED_EDGE('',*,*,#1579,.F.);
#2079=ORIENTED_EDGE('',*,*,#1581,.F.);
#2080=ORIENTED_EDGE('',*,*,#1582,.T.);
#2081=ORIENTED_EDGE('',*,*,#1583,.T.);
#2082=ORIENTED_EDGE('',*,*,#1582,.F.);
#2083=ORIENTED_EDGE('',*,*,#1578,.T.);
#2084=ORIENTED_EDGE('',*,*,#1581,.T.);
#2085=ORIENTED_EDGE('',*,*,#1584,.F.);
#2086=ORIENTED_EDGE('',*,*,#1585,.T.);
#2087=ORIENTED_EDGE('',*,*,#1586,.T.);
#2088=ORIENTED_EDGE('',*,*,#1585,.F.);
#2089=ORIENTED_EDGE('',*,*,#1584,.T.);
#2090=ORIENTED_EDGE('',*,*,#1580,.T.);
#2091=ORIENTED_EDGE('',*,*,#1586,.F.);
#2092=ORIENTED_EDGE('',*,*,#1583,.F.);
#2093=ORIENTED_EDGE('',*,*,#1587,.F.);
#2094=ORIENTED_EDGE('',*,*,#1588,.T.);
#2095=ORIENTED_EDGE('',*,*,#1589,.F.);
#2096=ORIENTED_EDGE('',*,*,#1590,.F.);
#2097=ORIENTED_EDGE('',*,*,#1589,.T.);
#2098=ORIENTED_EDGE('',*,*,#1591,.T.);
#2099=ORIENTED_EDGE('',*,*,#1592,.T.);
#2100=ORIENTED_EDGE('',*,*,#1593,.T.);
#2101=ORIENTED_EDGE('',*,*,#1587,.T.);
#2102=ORIENTED_EDGE('',*,*,#1594,.T.);
#2103=ORIENTED_EDGE('',*,*,#1595,.T.);
#2104=ORIENTED_EDGE('',*,*,#1596,.F.);
#2105=ORIENTED_EDGE('',*,*,#1595,.F.);
#2106=ORIENTED_EDGE('',*,*,#1597,.T.);
#2107=ORIENTED_EDGE('',*,*,#1598,.F.);
#2108=ORIENTED_EDGE('',*,*,#1599,.F.);
#2109=ORIENTED_EDGE('',*,*,#1598,.T.);
#2110=ORIENTED_EDGE('',*,*,#1600,.T.);
#2111=ORIENTED_EDGE('',*,*,#1601,.T.);
#2112=ORIENTED_EDGE('',*,*,#1602,.T.);
#2113=ORIENTED_EDGE('',*,*,#1603,.T.);
#2114=ORIENTED_EDGE('',*,*,#1592,.F.);
#2115=ORIENTED_EDGE('',*,*,#1604,.F.);
#2116=ORIENTED_EDGE('',*,*,#1605,.F.);
#2117=ORIENTED_EDGE('',*,*,#1606,.T.);
#2118=ORIENTED_EDGE('',*,*,#1605,.T.);
#2119=ORIENTED_EDGE('',*,*,#1607,.F.);
#2120=ORIENTED_EDGE('',*,*,#1608,.F.);
#2121=ORIENTED_EDGE('',*,*,#1609,.T.);
#2122=ORIENTED_EDGE('',*,*,#1608,.T.);
#2123=ORIENTED_EDGE('',*,*,#1610,.F.);
#2124=ORIENTED_EDGE('',*,*,#1611,.F.);
#2125=ORIENTED_EDGE('',*,*,#1612,.T.);
#2126=ORIENTED_EDGE('',*,*,#1611,.T.);
#2127=ORIENTED_EDGE('',*,*,#1613,.T.);
#2128=ORIENTED_EDGE('',*,*,#1601,.F.);
#2129=ORIENTED_EDGE('',*,*,#1613,.F.);
#2130=ORIENTED_EDGE('',*,*,#1610,.T.);
#2131=ORIENTED_EDGE('',*,*,#1607,.T.);
#2132=ORIENTED_EDGE('',*,*,#1604,.T.);
#2133=ORIENTED_EDGE('',*,*,#1591,.F.);
#2134=ORIENTED_EDGE('',*,*,#1588,.F.);
#2135=ORIENTED_EDGE('',*,*,#1596,.T.);
#2136=ORIENTED_EDGE('',*,*,#1599,.T.);
#2137=ORIENTED_EDGE('',*,*,#1602,.F.);
#2138=ORIENTED_EDGE('',*,*,#1612,.F.);
#2139=ORIENTED_EDGE('',*,*,#1600,.F.);
#2140=ORIENTED_EDGE('',*,*,#1597,.F.);
#2141=ORIENTED_EDGE('',*,*,#1594,.F.);
#2142=ORIENTED_EDGE('',*,*,#1590,.T.);
#2143=ORIENTED_EDGE('',*,*,#1593,.F.);
#2144=ORIENTED_EDGE('',*,*,#1603,.F.);
#2145=ORIENTED_EDGE('',*,*,#1606,.F.);
#2146=ORIENTED_EDGE('',*,*,#1609,.F.);
#2147=ORIENTED_EDGE('',*,*,#1614,.F.);
#2148=ORIENTED_EDGE('',*,*,#1615,.T.);
#2149=ORIENTED_EDGE('',*,*,#1616,.F.);
#2150=ORIENTED_EDGE('',*,*,#1617,.F.);
#2151=ORIENTED_EDGE('',*,*,#1615,.F.);
#2152=ORIENTED_EDGE('',*,*,#1618,.F.);
#2153=ORIENTED_EDGE('',*,*,#1619,.F.);
#2154=ORIENTED_EDGE('',*,*,#1620,.T.);
#2155=ORIENTED_EDGE('',*,*,#1621,.F.);
#2156=ORIENTED_EDGE('',*,*,#1620,.F.);
#2157=ORIENTED_EDGE('',*,*,#1622,.F.);
#2158=ORIENTED_EDGE('',*,*,#1623,.T.);
#2159=ORIENTED_EDGE('',*,*,#1624,.F.);
#2160=ORIENTED_EDGE('',*,*,#1623,.F.);
#2161=ORIENTED_EDGE('',*,*,#1625,.F.);
#2162=ORIENTED_EDGE('',*,*,#1626,.T.);
#2163=ORIENTED_EDGE('',*,*,#1627,.F.);
#2164=ORIENTED_EDGE('',*,*,#1626,.F.);
#2165=ORIENTED_EDGE('',*,*,#1628,.F.);
#2166=ORIENTED_EDGE('',*,*,#1629,.T.);
#2167=ORIENTED_EDGE('',*,*,#1630,.F.);
#2168=ORIENTED_EDGE('',*,*,#1631,.F.);
#2169=ORIENTED_EDGE('',*,*,#1629,.F.);
#2170=ORIENTED_EDGE('',*,*,#1632,.F.);
#2171=ORIENTED_EDGE('',*,*,#1633,.F.);
#2172=ORIENTED_EDGE('',*,*,#1634,.T.);
#2173=ORIENTED_EDGE('',*,*,#1635,.F.);
#2174=ORIENTED_EDGE('',*,*,#1634,.F.);
#2175=ORIENTED_EDGE('',*,*,#1636,.F.);
#2176=ORIENTED_EDGE('',*,*,#1637,.T.);
#2177=ORIENTED_EDGE('',*,*,#1638,.F.);
#2178=ORIENTED_EDGE('',*,*,#1637,.F.);
#2179=ORIENTED_EDGE('',*,*,#1639,.F.);
#2180=ORIENTED_EDGE('',*,*,#1640,.T.);
#2181=ORIENTED_EDGE('',*,*,#1641,.F.);
#2182=ORIENTED_EDGE('',*,*,#1640,.F.);
#2183=ORIENTED_EDGE('',*,*,#1642,.F.);
#2184=ORIENTED_EDGE('',*,*,#1643,.F.);
#2185=ORIENTED_EDGE('',*,*,#1644,.F.);
#2186=ORIENTED_EDGE('',*,*,#1645,.T.);
#2187=ORIENTED_EDGE('',*,*,#1646,.T.);
#2188=ORIENTED_EDGE('',*,*,#1643,.T.);
#2189=ORIENTED_EDGE('',*,*,#1647,.T.);
#2190=ORIENTED_EDGE('',*,*,#1648,.F.);
#2191=ORIENTED_EDGE('',*,*,#1649,.F.);
#2192=ORIENTED_EDGE('',*,*,#1650,.F.);
#2193=ORIENTED_EDGE('',*,*,#1651,.T.);
#2194=ORIENTED_EDGE('',*,*,#1652,.T.);
#2195=ORIENTED_EDGE('',*,*,#1649,.T.);
#2196=ORIENTED_EDGE('',*,*,#1653,.T.);
#2197=ORIENTED_EDGE('',*,*,#1654,.F.);
#2198=ORIENTED_EDGE('',*,*,#1655,.F.);
#2199=ORIENTED_EDGE('',*,*,#1656,.F.);
#2200=ORIENTED_EDGE('',*,*,#1657,.T.);
#2201=ORIENTED_EDGE('',*,*,#1658,.T.);
#2202=ORIENTED_EDGE('',*,*,#1655,.T.);
#2203=ORIENTED_EDGE('',*,*,#1659,.T.);
#2204=ORIENTED_EDGE('',*,*,#1642,.T.);
#2205=ORIENTED_EDGE('',*,*,#1660,.T.);
#2206=ORIENTED_EDGE('',*,*,#1656,.T.);
#2207=ORIENTED_EDGE('',*,*,#1661,.T.);
#2208=ORIENTED_EDGE('',*,*,#1662,.F.);
#2209=ORIENTED_EDGE('',*,*,#1663,.F.);
#2210=ORIENTED_EDGE('',*,*,#1664,.F.);
#2211=ORIENTED_EDGE('',*,*,#1665,.T.);
#2212=ORIENTED_EDGE('',*,*,#1666,.T.);
#2213=ORIENTED_EDGE('',*,*,#1663,.T.);
#2214=ORIENTED_EDGE('',*,*,#1667,.T.);
#2215=ORIENTED_EDGE('',*,*,#1654,.T.);
#2216=ORIENTED_EDGE('',*,*,#1668,.T.);
#2217=ORIENTED_EDGE('',*,*,#1664,.T.);
#2218=ORIENTED_EDGE('',*,*,#1669,.T.);
#2219=ORIENTED_EDGE('',*,*,#1662,.T.);
#2220=ORIENTED_EDGE('',*,*,#1670,.T.);
#2221=ORIENTED_EDGE('',*,*,#1650,.T.);
#2222=ORIENTED_EDGE('',*,*,#1671,.T.);
#2223=ORIENTED_EDGE('',*,*,#1648,.T.);
#2224=ORIENTED_EDGE('',*,*,#1672,.T.);
#2225=ORIENTED_EDGE('',*,*,#1644,.T.);
#2226=ORIENTED_EDGE('',*,*,#1673,.T.);
#2227=ORIENTED_EDGE('',*,*,#1647,.F.);
#2228=ORIENTED_EDGE('',*,*,#1661,.F.);
#2229=ORIENTED_EDGE('',*,*,#1658,.F.);
#2230=ORIENTED_EDGE('',*,*,#1674,.T.);
#2231=ORIENTED_EDGE('',*,*,#1675,.T.);
#2232=ORIENTED_EDGE('',*,*,#1676,.T.);
#2233=ORIENTED_EDGE('',*,*,#1677,.T.);
#2234=ORIENTED_EDGE('',*,*,#1678,.T.);
#2235=ORIENTED_EDGE('',*,*,#1679,.T.);
#2236=ORIENTED_EDGE('',*,*,#1680,.F.);
#2237=ORIENTED_EDGE('',*,*,#1681,.T.);
#2238=ORIENTED_EDGE('',*,*,#1682,.T.);
#2239=ORIENTED_EDGE('',*,*,#1683,.T.);
#2240=ORIENTED_EDGE('',*,*,#1684,.T.);
#2241=ORIENTED_EDGE('',*,*,#1685,.T.);
#2242=ORIENTED_EDGE('',*,*,#1686,.T.);
#2243=ORIENTED_EDGE('',*,*,#1687,.T.);
#2244=ORIENTED_EDGE('',*,*,#1659,.F.);
#2245=ORIENTED_EDGE('',*,*,#1669,.F.);
#2246=ORIENTED_EDGE('',*,*,#1666,.F.);
#2247=ORIENTED_EDGE('',*,*,#1688,.T.);
#2248=ORIENTED_EDGE('',*,*,#1657,.F.);
#2249=ORIENTED_EDGE('',*,*,#1688,.F.);
#2250=ORIENTED_EDGE('',*,*,#1665,.F.);
#2251=ORIENTED_EDGE('',*,*,#1689,.F.);
#2252=ORIENTED_EDGE('',*,*,#1690,.T.);
#2253=ORIENTED_EDGE('',*,*,#1674,.F.);
#2254=ORIENTED_EDGE('',*,*,#1660,.F.);
#2255=ORIENTED_EDGE('',*,*,#1672,.F.);
#2256=ORIENTED_EDGE('',*,*,#1670,.F.);
#2257=ORIENTED_EDGE('',*,*,#1668,.F.);
#2258=ORIENTED_EDGE('',*,*,#1639,.T.);
#2259=ORIENTED_EDGE('',*,*,#1636,.T.);
#2260=ORIENTED_EDGE('',*,*,#1628,.T.);
#2261=ORIENTED_EDGE('',*,*,#1625,.T.);
#2262=ORIENTED_EDGE('',*,*,#1622,.T.);
#2263=ORIENTED_EDGE('',*,*,#1614,.T.);
#2264=ORIENTED_EDGE('',*,*,#1687,.F.);
#2265=ORIENTED_EDGE('',*,*,#1691,.T.);
#2266=ORIENTED_EDGE('',*,*,#1692,.F.);
#2267=ORIENTED_EDGE('',*,*,#1691,.F.);
#2268=ORIENTED_EDGE('',*,*,#1618,.T.);
#2269=ORIENTED_EDGE('',*,*,#1619,.T.);
#2270=ORIENTED_EDGE('',*,*,#1616,.T.);
#2271=ORIENTED_EDGE('',*,*,#1617,.T.);
#2272=ORIENTED_EDGE('',*,*,#1632,.T.);
#2273=ORIENTED_EDGE('',*,*,#1633,.T.);
#2274=ORIENTED_EDGE('',*,*,#1630,.T.);
#2275=ORIENTED_EDGE('',*,*,#1631,.T.);
#2276=ORIENTED_EDGE('',*,*,#1693,.F.);
#2277=ORIENTED_EDGE('',*,*,#1694,.T.);
#2278=ORIENTED_EDGE('',*,*,#1683,.F.);
#2279=ORIENTED_EDGE('',*,*,#1695,.F.);
#2280=ORIENTED_EDGE('',*,*,#1696,.F.);
#2281=ORIENTED_EDGE('',*,*,#1697,.F.);
#2282=ORIENTED_EDGE('',*,*,#1685,.F.);
#2283=ORIENTED_EDGE('',*,*,#1698,.T.);
#2284=ORIENTED_EDGE('',*,*,#1699,.F.);
#2285=ORIENTED_EDGE('',*,*,#1698,.F.);
#2286=ORIENTED_EDGE('',*,*,#1684,.F.);
#2287=ORIENTED_EDGE('',*,*,#1694,.F.);
#2288=ORIENTED_EDGE('',*,*,#1624,.T.);
#2289=ORIENTED_EDGE('',*,*,#1638,.T.);
#2290=ORIENTED_EDGE('',*,*,#1700,.F.);
#2291=ORIENTED_EDGE('',*,*,#1701,.T.);
#2292=ORIENTED_EDGE('',*,*,#1675,.F.);
#2293=ORIENTED_EDGE('',*,*,#1690,.F.);
#2294=ORIENTED_EDGE('',*,*,#1702,.F.);
#2295=ORIENTED_EDGE('',*,*,#1703,.F.);
#2296=ORIENTED_EDGE('',*,*,#1677,.F.);
#2297=ORIENTED_EDGE('',*,*,#1704,.T.);
#2298=ORIENTED_EDGE('',*,*,#1705,.F.);
#2299=ORIENTED_EDGE('',*,*,#1704,.F.);
#2300=ORIENTED_EDGE('',*,*,#1676,.F.);
#2301=ORIENTED_EDGE('',*,*,#1701,.F.);
#2302=ORIENTED_EDGE('',*,*,#1627,.T.);
#2303=ORIENTED_EDGE('',*,*,#1641,.T.);
#2304=ORIENTED_EDGE('',*,*,#1645,.F.);
#2305=ORIENTED_EDGE('',*,*,#1686,.F.);
#2306=ORIENTED_EDGE('',*,*,#1697,.T.);
#2307=ORIENTED_EDGE('',*,*,#1706,.F.);
#2308=ORIENTED_EDGE('',*,*,#1651,.F.);
#2309=ORIENTED_EDGE('',*,*,#1707,.F.);
#2310=ORIENTED_EDGE('',*,*,#1703,.T.);
#2311=ORIENTED_EDGE('',*,*,#1708,.F.);
#2312=ORIENTED_EDGE('',*,*,#1709,.F.);
#2313=ORIENTED_EDGE('',*,*,#1678,.F.);
#2314=ORIENTED_EDGE('',*,*,#1695,.T.);
#2315=ORIENTED_EDGE('',*,*,#1682,.F.);
#2316=ORIENTED_EDGE('',*,*,#1710,.F.);
#2317=ORIENTED_EDGE('',*,*,#1711,.F.);
#2318=ORIENTED_EDGE('',*,*,#1712,.F.);
#2319=ORIENTED_EDGE('',*,*,#1710,.T.);
#2320=ORIENTED_EDGE('',*,*,#1681,.F.);
#2321=ORIENTED_EDGE('',*,*,#1713,.F.);
#2322=ORIENTED_EDGE('',*,*,#1714,.F.);
#2323=ORIENTED_EDGE('',*,*,#1715,.F.);
#2324=ORIENTED_EDGE('',*,*,#1679,.F.);
#2325=ORIENTED_EDGE('',*,*,#1709,.T.);
#2326=ORIENTED_EDGE('',*,*,#1652,.F.);
#2327=ORIENTED_EDGE('',*,*,#1706,.T.);
#2328=ORIENTED_EDGE('',*,*,#1696,.T.);
#2329=ORIENTED_EDGE('',*,*,#1699,.T.);
#2330=ORIENTED_EDGE('',*,*,#1693,.T.);
#2331=ORIENTED_EDGE('',*,*,#1711,.T.);
#2332=ORIENTED_EDGE('',*,*,#1712,.T.);
#2333=ORIENTED_EDGE('',*,*,#1716,.F.);
#2334=ORIENTED_EDGE('',*,*,#1714,.T.);
#2335=ORIENTED_EDGE('',*,*,#1708,.T.);
#2336=ORIENTED_EDGE('',*,*,#1702,.T.);
#2337=ORIENTED_EDGE('',*,*,#1705,.T.);
#2338=ORIENTED_EDGE('',*,*,#1700,.T.);
#2339=ORIENTED_EDGE('',*,*,#1689,.T.);
#2340=ORIENTED_EDGE('',*,*,#1667,.F.);
#2341=ORIENTED_EDGE('',*,*,#1671,.F.);
#2342=ORIENTED_EDGE('',*,*,#1692,.T.);
#2343=ORIENTED_EDGE('',*,*,#1713,.T.);
#2344=ORIENTED_EDGE('',*,*,#1680,.T.);
#2345=ORIENTED_EDGE('',*,*,#1715,.T.);
#2346=ORIENTED_EDGE('',*,*,#1716,.T.);
#2347=ORIENTED_EDGE('',*,*,#1621,.T.);
#2348=ORIENTED_EDGE('',*,*,#1635,.T.);
#2349=ORIENTED_EDGE('',*,*,#1646,.F.);
#2350=ORIENTED_EDGE('',*,*,#1707,.T.);
#2351=ORIENTED_EDGE('',*,*,#1653,.F.);
#2352=ORIENTED_EDGE('',*,*,#1673,.F.);
#2353=ORIENTED_EDGE('',*,*,#1717,.F.);
#2354=ORIENTED_EDGE('',*,*,#1718,.T.);
#2355=ORIENTED_EDGE('',*,*,#1719,.F.);
#2356=ORIENTED_EDGE('',*,*,#1718,.F.);
#2357=ORIENTED_EDGE('',*,*,#1717,.T.);
#2358=ORIENTED_EDGE('',*,*,#1720,.T.);
#2359=ORIENTED_EDGE('',*,*,#1721,.T.);
#2360=ORIENTED_EDGE('',*,*,#1722,.T.);
#2361=ORIENTED_EDGE('',*,*,#1723,.T.);
#2362=ORIENTED_EDGE('',*,*,#1722,.F.);
#2363=ORIENTED_EDGE('',*,*,#1724,.T.);
#2364=ORIENTED_EDGE('',*,*,#1725,.F.);
#2365=ORIENTED_EDGE('',*,*,#1726,.T.);
#2366=ORIENTED_EDGE('',*,*,#1727,.F.);
#2367=ORIENTED_EDGE('',*,*,#1728,.T.);
#2368=ORIENTED_EDGE('',*,*,#1729,.F.);
#2369=ORIENTED_EDGE('',*,*,#1730,.T.);
#2370=ORIENTED_EDGE('',*,*,#1721,.F.);
#2371=ORIENTED_EDGE('',*,*,#1731,.F.);
#2372=ORIENTED_EDGE('',*,*,#1732,.F.);
#2373=ORIENTED_EDGE('',*,*,#1724,.F.);
#2374=ORIENTED_EDGE('',*,*,#1733,.T.);
#2375=ORIENTED_EDGE('',*,*,#1734,.T.);
#2376=ORIENTED_EDGE('',*,*,#1725,.T.);
#2377=ORIENTED_EDGE('',*,*,#1732,.T.);
#2378=ORIENTED_EDGE('',*,*,#1735,.T.);
#2379=ORIENTED_EDGE('',*,*,#1736,.T.);
#2380=ORIENTED_EDGE('',*,*,#1729,.T.);
#2381=ORIENTED_EDGE('',*,*,#1737,.T.);
#2382=ORIENTED_EDGE('',*,*,#1737,.F.);
#2383=ORIENTED_EDGE('',*,*,#1728,.F.);
#2384=ORIENTED_EDGE('',*,*,#1738,.F.);
#2385=ORIENTED_EDGE('',*,*,#1739,.F.);
#2386=ORIENTED_EDGE('',*,*,#1740,.T.);
#2387=ORIENTED_EDGE('',*,*,#1738,.T.);
#2388=ORIENTED_EDGE('',*,*,#1727,.T.);
#2389=ORIENTED_EDGE('',*,*,#1741,.T.);
#2390=ORIENTED_EDGE('',*,*,#1734,.F.);
#2391=ORIENTED_EDGE('',*,*,#1742,.F.);
#2392=ORIENTED_EDGE('',*,*,#1741,.F.);
#2393=ORIENTED_EDGE('',*,*,#1726,.F.);
#2394=ORIENTED_EDGE('',*,*,#1723,.F.);
#2395=ORIENTED_EDGE('',*,*,#1730,.F.);
#2396=ORIENTED_EDGE('',*,*,#1736,.F.);
#2397=ORIENTED_EDGE('',*,*,#1743,.F.);
#2398=ORIENTED_EDGE('',*,*,#1720,.F.);
#2399=ORIENTED_EDGE('',*,*,#1743,.T.);
#2400=ORIENTED_EDGE('',*,*,#1735,.F.);
#2401=ORIENTED_EDGE('',*,*,#1739,.T.);
#2402=ORIENTED_EDGE('',*,*,#1740,.F.);
#2403=ORIENTED_EDGE('',*,*,#1742,.T.);
#2404=ORIENTED_EDGE('',*,*,#1733,.F.);
#2405=ORIENTED_EDGE('',*,*,#1731,.T.);
#2406=ORIENTED_EDGE('',*,*,#1719,.T.);
#2407=ORIENTED_EDGE('',*,*,#1744,.T.);
#2408=ORIENTED_EDGE('',*,*,#1745,.T.);
#2409=ORIENTED_EDGE('',*,*,#1746,.T.);
#2410=ORIENTED_EDGE('',*,*,#1745,.F.);
#2411=ORIENTED_EDGE('',*,*,#1747,.T.);
#2412=ORIENTED_EDGE('',*,*,#1748,.T.);
#2413=ORIENTED_EDGE('',*,*,#1749,.F.);
#2414=ORIENTED_EDGE('',*,*,#1748,.F.);
#2415=ORIENTED_EDGE('',*,*,#1744,.F.);
#2416=ORIENTED_EDGE('',*,*,#1747,.F.);
#2417=ORIENTED_EDGE('',*,*,#1750,.T.);
#2418=ORIENTED_EDGE('',*,*,#1751,.T.);
#2419=ORIENTED_EDGE('',*,*,#1752,.F.);
#2420=ORIENTED_EDGE('',*,*,#1751,.F.);
#2421=ORIENTED_EDGE('',*,*,#1750,.F.);
#2422=ORIENTED_EDGE('',*,*,#1746,.F.);
#2423=ORIENTED_EDGE('',*,*,#1752,.T.);
#2424=ORIENTED_EDGE('',*,*,#1749,.T.);
#2425=ORIENTED_EDGE('',*,*,#1753,.T.);
#2426=ORIENTED_EDGE('',*,*,#1754,.T.);
#2427=ORIENTED_EDGE('',*,*,#1755,.T.);
#2428=ORIENTED_EDGE('',*,*,#1756,.T.);
#2429=ORIENTED_EDGE('',*,*,#1754,.F.);
#2430=ORIENTED_EDGE('',*,*,#1757,.F.);
#2431=ORIENTED_EDGE('',*,*,#1758,.F.);
#2432=ORIENTED_EDGE('',*,*,#1759,.T.);
#2433=ORIENTED_EDGE('',*,*,#1753,.F.);
#2434=ORIENTED_EDGE('',*,*,#1760,.T.);
#2435=ORIENTED_EDGE('',*,*,#1761,.F.);
#2436=ORIENTED_EDGE('',*,*,#1762,.T.);
#2437=ORIENTED_EDGE('',*,*,#1763,.F.);
#2438=ORIENTED_EDGE('',*,*,#1764,.T.);
#2439=ORIENTED_EDGE('',*,*,#1765,.F.);
#2440=ORIENTED_EDGE('',*,*,#1757,.T.);
#2441=ORIENTED_EDGE('',*,*,#1765,.T.);
#2442=ORIENTED_EDGE('',*,*,#1766,.T.);
#2443=ORIENTED_EDGE('',*,*,#1767,.T.);
#2444=ORIENTED_EDGE('',*,*,#1758,.T.);
#2445=ORIENTED_EDGE('',*,*,#1766,.F.);
#2446=ORIENTED_EDGE('',*,*,#1764,.F.);
#2447=ORIENTED_EDGE('',*,*,#1768,.F.);
#2448=ORIENTED_EDGE('',*,*,#1769,.T.);
#2449=ORIENTED_EDGE('',*,*,#1761,.T.);
#2450=ORIENTED_EDGE('',*,*,#1770,.T.);
#2451=ORIENTED_EDGE('',*,*,#1771,.T.);
#2452=ORIENTED_EDGE('',*,*,#1772,.T.);
#2453=ORIENTED_EDGE('',*,*,#1756,.F.);
#2454=ORIENTED_EDGE('',*,*,#1773,.T.);
#2455=ORIENTED_EDGE('',*,*,#1770,.F.);
#2456=ORIENTED_EDGE('',*,*,#1760,.F.);
#2457=ORIENTED_EDGE('',*,*,#1763,.T.);
#2458=ORIENTED_EDGE('',*,*,#1774,.T.);
#2459=ORIENTED_EDGE('',*,*,#1775,.T.);
#2460=ORIENTED_EDGE('',*,*,#1768,.T.);
#2461=ORIENTED_EDGE('',*,*,#1772,.F.);
#2462=ORIENTED_EDGE('',*,*,#1776,.T.);
#2463=ORIENTED_EDGE('',*,*,#1774,.F.);
#2464=ORIENTED_EDGE('',*,*,#1762,.F.);
#2465=ORIENTED_EDGE('',*,*,#1755,.F.);
#2466=ORIENTED_EDGE('',*,*,#1759,.F.);
#2467=ORIENTED_EDGE('',*,*,#1767,.F.);
#2468=ORIENTED_EDGE('',*,*,#1769,.F.);
#2469=ORIENTED_EDGE('',*,*,#1775,.F.);
#2470=ORIENTED_EDGE('',*,*,#1776,.F.);
#2471=ORIENTED_EDGE('',*,*,#1771,.F.);
#2472=ORIENTED_EDGE('',*,*,#1773,.F.);
#2473=CYLINDRICAL_SURFACE('',#2822,4.);
#2474=CYLINDRICAL_SURFACE('',#2826,4.);
#2475=CYLINDRICAL_SURFACE('',#2830,4.);
#2476=CYLINDRICAL_SURFACE('',#2834,4.);
#2477=CYLINDRICAL_SURFACE('',#2838,4.);
#2478=CYLINDRICAL_SURFACE('',#2842,4.);
#2479=CYLINDRICAL_SURFACE('',#2853,4.);
#2480=CYLINDRICAL_SURFACE('',#2857,4.);
#2481=CYLINDRICAL_SURFACE('',#2861,4.);
#2482=CYLINDRICAL_SURFACE('',#2865,4.);
#2483=CYLINDRICAL_SURFACE('',#2869,4.);
#2484=CYLINDRICAL_SURFACE('',#2873,4.);
#2485=CYLINDRICAL_SURFACE('',#2884,6.);
#2486=CYLINDRICAL_SURFACE('',#2890,1.);
#2487=CYLINDRICAL_SURFACE('',#2893,1.);
#2488=CYLINDRICAL_SURFACE('',#2895,1.);
#2489=CYLINDRICAL_SURFACE('',#2897,1.);
#2490=CYLINDRICAL_SURFACE('',#2900,1.);
#2491=CYLINDRICAL_SURFACE('',#2902,1.);
#2492=CYLINDRICAL_SURFACE('',#2903,1.);
#2493=CYLINDRICAL_SURFACE('',#2905,1.);
#2494=CYLINDRICAL_SURFACE('',#2917,1.);
#2495=CYLINDRICAL_SURFACE('',#2920,1.);
#2496=CYLINDRICAL_SURFACE('',#2922,1.);
#2497=CYLINDRICAL_SURFACE('',#2925,1.);
#2498=CYLINDRICAL_SURFACE('',#2926,1.);
#2499=CYLINDRICAL_SURFACE('',#2928,1.);
#2500=CYLINDRICAL_SURFACE('',#2930,1.);
#2501=CYLINDRICAL_SURFACE('',#2932,1.);
#2502=CYLINDRICAL_SURFACE('',#2946,7.);
#2503=CYLINDRICAL_SURFACE('',#2949,6.);
#2504=CYLINDRICAL_SURFACE('',#2953,11.);
#2505=CYLINDRICAL_SURFACE('',#2971,5.);
#2506=CYLINDRICAL_SURFACE('',#2973,5.);
#2507=CYLINDRICAL_SURFACE('',#2975,5.);
#2508=CYLINDRICAL_SURFACE('',#2978,5.);
#2509=CYLINDRICAL_SURFACE('',#2981,5.);
#2510=CYLINDRICAL_SURFACE('',#2983,5.);
#2511=CYLINDRICAL_SURFACE('',#2985,5.);
#2512=CYLINDRICAL_SURFACE('',#2988,5.);
#2513=CYLINDRICAL_SURFACE('',#2995,1.);
#2514=CYLINDRICAL_SURFACE('',#3001,1.);
#2515=CYLINDRICAL_SURFACE('',#3007,1.);
#2516=CYLINDRICAL_SURFACE('',#3009,1.);
#2517=CYLINDRICAL_SURFACE('',#3014,1.);
#2518=CYLINDRICAL_SURFACE('',#3016,1.);
#2519=CYLINDRICAL_SURFACE('',#3017,1.);
#2520=CYLINDRICAL_SURFACE('',#3018,1.);
#2521=CYLINDRICAL_SURFACE('',#3024,6.);
#2522=CYLINDRICAL_SURFACE('',#3041,17.5);
#2523=CYLINDRICAL_SURFACE('',#3056,7.);
#2524=CYLINDRICAL_SURFACE('',#3059,6.);
#2525=CYLINDRICAL_SURFACE('',#3063,11.);
#2526=ADVANCED_FACE('',(#268),#2473,.F.);
#2527=ADVANCED_FACE('',(#269),#164,.T.);
#2528=ADVANCED_FACE('',(#270),#2474,.F.);
#2529=ADVANCED_FACE('',(#271),#165,.T.);
#2530=ADVANCED_FACE('',(#272),#2475,.F.);
#2531=ADVANCED_FACE('',(#273),#166,.T.);
#2532=ADVANCED_FACE('',(#274),#2476,.F.);
#2533=ADVANCED_FACE('',(#275),#167,.T.);
#2534=ADVANCED_FACE('',(#276),#2477,.F.);
#2535=ADVANCED_FACE('',(#277),#168,.T.);
#2536=ADVANCED_FACE('',(#278),#2478,.F.);
#2537=ADVANCED_FACE('',(#279),#169,.T.);
#2538=ADVANCED_FACE('',(#280),#170,.T.);
#2539=ADVANCED_FACE('',(#281),#171,.T.);
#2540=ADVANCED_FACE('',(#282),#172,.T.);
#2541=ADVANCED_FACE('',(#283),#173,.T.);
#2542=ADVANCED_FACE('',(#284,#127,#128,#129,#130,#131,#132),#174,.T.);
#2543=ADVANCED_FACE('',(#285),#175,.F.);
#2544=ADVANCED_FACE('',(#286),#2479,.F.);
#2545=ADVANCED_FACE('',(#287),#176,.T.);
#2546=ADVANCED_FACE('',(#288),#2480,.F.);
#2547=ADVANCED_FACE('',(#289),#177,.T.);
#2548=ADVANCED_FACE('',(#290),#2481,.F.);
#2549=ADVANCED_FACE('',(#291),#178,.T.);
#2550=ADVANCED_FACE('',(#292),#2482,.F.);
#2551=ADVANCED_FACE('',(#293),#179,.T.);
#2552=ADVANCED_FACE('',(#294),#2483,.F.);
#2553=ADVANCED_FACE('',(#295),#180,.T.);
#2554=ADVANCED_FACE('',(#296),#2484,.F.);
#2555=ADVANCED_FACE('',(#297),#181,.T.);
#2556=ADVANCED_FACE('',(#298),#182,.T.);
#2557=ADVANCED_FACE('',(#299),#183,.T.);
#2558=ADVANCED_FACE('',(#300),#184,.T.);
#2559=ADVANCED_FACE('',(#301),#185,.T.);
#2560=ADVANCED_FACE('',(#302,#133,#134,#135,#136,#137,#138),#186,.T.);
#2561=ADVANCED_FACE('',(#303),#187,.F.);
#2562=ADVANCED_FACE('',(#304),#2485,.T.);
#2563=ADVANCED_FACE('',(#305),#188,.T.);
#2564=ADVANCED_FACE('',(#306),#189,.F.);
#2565=ADVANCED_FACE('',(#307),#2486,.T.);
#2566=ADVANCED_FACE('',(#308),#2487,.T.);
#2567=ADVANCED_FACE('',(#309),#2488,.T.);
#2568=ADVANCED_FACE('',(#310),#2489,.T.);
#2569=ADVANCED_FACE('',(#311),#2490,.T.);
#2570=ADVANCED_FACE('',(#312),#2491,.T.);
#2571=ADVANCED_FACE('',(#313),#2492,.T.);
#2572=ADVANCED_FACE('',(#314),#2493,.T.);
#2573=ADVANCED_FACE('',(#315),#190,.F.);
#2574=ADVANCED_FACE('',(#316),#191,.F.);
#2575=ADVANCED_FACE('',(#317),#192,.F.);
#2576=ADVANCED_FACE('',(#318),#193,.F.);
#2577=ADVANCED_FACE('',(#319),#194,.F.);
#2578=ADVANCED_FACE('',(#320),#195,.F.);
#2579=ADVANCED_FACE('',(#321),#196,.F.);
#2580=ADVANCED_FACE('',(#322),#197,.F.);
#2581=ADVANCED_FACE('',(#323),#198,.F.);
#2582=ADVANCED_FACE('',(#324),#199,.T.);
#2583=ADVANCED_FACE('',(#325),#2494,.T.);
#2584=ADVANCED_FACE('',(#326),#2495,.T.);
#2585=ADVANCED_FACE('',(#327),#2496,.T.);
#2586=ADVANCED_FACE('',(#328),#2497,.T.);
#2587=ADVANCED_FACE('',(#329),#2498,.T.);
#2588=ADVANCED_FACE('',(#330),#2499,.T.);
#2589=ADVANCED_FACE('',(#331),#2500,.T.);
#2590=ADVANCED_FACE('',(#332),#2501,.T.);
#2591=ADVANCED_FACE('',(#333),#200,.T.);
#2592=ADVANCED_FACE('',(#334),#201,.T.);
#2593=ADVANCED_FACE('',(#335),#202,.T.);
#2594=ADVANCED_FACE('',(#336),#203,.T.);
#2595=ADVANCED_FACE('',(#337),#204,.F.);
#2596=ADVANCED_FACE('',(#338),#205,.F.);
#2597=ADVANCED_FACE('',(#339),#206,.F.);
#2598=ADVANCED_FACE('',(#340),#207,.T.);
#2599=ADVANCED_FACE('',(#341),#208,.T.);
#2600=ADVANCED_FACE('',(#342),#209,.T.);
#2601=ADVANCED_FACE('',(#343),#210,.T.);
#2602=ADVANCED_FACE('',(#344),#211,.T.);
#2603=ADVANCED_FACE('',(#345),#2502,.T.);
#2604=ADVANCED_FACE('',(#346),#2503,.F.);
#2605=ADVANCED_FACE('',(#347,#139),#212,.T.);
#2606=ADVANCED_FACE('',(#348),#2504,.T.);
#2607=ADVANCED_FACE('',(#349,#140),#213,.T.);
#2608=ADVANCED_FACE('',(#350,#141),#214,.F.);
#2609=ADVANCED_FACE('',(#351),#215,.T.);
#2610=ADVANCED_FACE('',(#352),#216,.T.);
#2611=ADVANCED_FACE('',(#353),#217,.T.);
#2612=ADVANCED_FACE('',(#354),#218,.T.);
#2613=ADVANCED_FACE('',(#355),#219,.T.);
#2614=ADVANCED_FACE('',(#356),#220,.T.);
#2615=ADVANCED_FACE('',(#357),#221,.T.);
#2616=ADVANCED_FACE('',(#358),#222,.T.);
#2617=ADVANCED_FACE('',(#359),#223,.T.);
#2618=ADVANCED_FACE('',(#360),#224,.T.);
#2619=ADVANCED_FACE('',(#361),#225,.F.);
#2620=ADVANCED_FACE('',(#362),#2505,.F.);
#2621=ADVANCED_FACE('',(#363),#2506,.F.);
#2622=ADVANCED_FACE('',(#364),#2507,.F.);
#2623=ADVANCED_FACE('',(#365),#2508,.F.);
#2624=ADVANCED_FACE('',(#366),#2509,.F.);
#2625=ADVANCED_FACE('',(#367),#2510,.F.);
#2626=ADVANCED_FACE('',(#368),#2511,.F.);
#2627=ADVANCED_FACE('',(#369),#2512,.F.);
#2628=ADVANCED_FACE('',(#370),#55,.T.);
#2629=ADVANCED_FACE('',(#371),#2513,.T.);
#2630=ADVANCED_FACE('',(#372),#56,.T.);
#2631=ADVANCED_FACE('',(#373),#2514,.T.);
#2632=ADVANCED_FACE('',(#374),#57,.T.);
#2633=ADVANCED_FACE('',(#375),#2515,.T.);
#2634=ADVANCED_FACE('',(#376),#2516,.T.);
#2635=ADVANCED_FACE('',(#377),#58,.T.);
#2636=ADVANCED_FACE('',(#378),#2517,.T.);
#2637=ADVANCED_FACE('',(#379),#2518,.T.);
#2638=ADVANCED_FACE('',(#380),#2519,.T.);
#2639=ADVANCED_FACE('',(#381),#2520,.T.);
#2640=ADVANCED_FACE('',(#382,#142),#226,.T.);
#2641=ADVANCED_FACE('',(#383),#227,.T.);
#2642=ADVANCED_FACE('',(#384),#228,.F.);
#2643=ADVANCED_FACE('',(#385,#143,#144,#145,#146,#147,#148),#229,.T.);
#2644=ADVANCED_FACE('',(#386,#149,#150,#151,#152),#2521,.F.);
#2645=ADVANCED_FACE('',(#387),#230,.F.);
#2646=ADVANCED_FACE('',(#388),#231,.F.);
#2647=ADVANCED_FACE('',(#389,#153,#154),#232,.F.);
#2648=ADVANCED_FACE('',(#390),#233,.F.);
#2649=ADVANCED_FACE('',(#391),#234,.F.);
#2650=ADVANCED_FACE('',(#392,#155,#156),#235,.F.);
#2651=ADVANCED_FACE('',(#393),#236,.F.);
#2652=ADVANCED_FACE('',(#394),#237,.F.);
#2653=ADVANCED_FACE('',(#395),#238,.F.);
#2654=ADVANCED_FACE('',(#396),#239,.F.);
#2655=ADVANCED_FACE('',(#397),#240,.F.);
#2656=ADVANCED_FACE('',(#398,#157),#241,.T.);
#2657=ADVANCED_FACE('',(#399,#158,#159),#242,.F.);
#2658=ADVANCED_FACE('',(#400),#243,.T.);
#2659=ADVANCED_FACE('',(#401),#2522,.T.);
#2660=ADVANCED_FACE('',(#402),#244,.T.);
#2661=ADVANCED_FACE('',(#403),#245,.T.);
#2662=ADVANCED_FACE('',(#404),#246,.F.);
#2663=ADVANCED_FACE('',(#405),#247,.T.);
#2664=ADVANCED_FACE('',(#406),#248,.T.);
#2665=ADVANCED_FACE('',(#407),#249,.T.);
#2666=ADVANCED_FACE('',(#408),#250,.T.);
#2667=ADVANCED_FACE('',(#409),#251,.T.);
#2668=ADVANCED_FACE('',(#410),#252,.T.);
#2669=ADVANCED_FACE('',(#411),#253,.T.);
#2670=ADVANCED_FACE('',(#412,#160),#254,.T.);
#2671=ADVANCED_FACE('',(#413),#2523,.T.);
#2672=ADVANCED_FACE('',(#414),#2524,.F.);
#2673=ADVANCED_FACE('',(#415,#161),#255,.F.);
#2674=ADVANCED_FACE('',(#416),#2525,.T.);
#2675=ADVANCED_FACE('',(#417,#162),#256,.F.);
#2676=ADVANCED_FACE('',(#418,#163),#257,.T.);
#2677=ADVANCED_FACE('',(#419),#258,.T.);
#2678=ADVANCED_FACE('',(#420),#259,.T.);
#2679=ADVANCED_FACE('',(#421),#260,.T.);
#2680=ADVANCED_FACE('',(#422),#261,.T.);
#2681=ADVANCED_FACE('',(#423),#262,.T.);
#2682=ADVANCED_FACE('',(#424),#263,.T.);
#2683=ADVANCED_FACE('',(#425),#264,.T.);
#2684=ADVANCED_FACE('',(#426),#265,.T.);
#2685=ADVANCED_FACE('',(#427),#266,.T.);
#2686=ADVANCED_FACE('',(#428),#267,.F.);
#2687=CLOSED_SHELL('',(#2526,#2527,#2528,#2529,#2530,#2531,#2532,#2533,
#2534,#2535,#2536,#2537,#2538,#2539,#2540,#2541,#2542,#2543));
#2688=CLOSED_SHELL('',(#2544,#2545,#2546,#2547,#2548,#2549,#2550,#2551,
#2552,#2553,#2554,#2555,#2556,#2557,#2558,#2559,#2560,#2561));
#2689=CLOSED_SHELL('',(#2562,#2563,#2564));
#2690=CLOSED_SHELL('',(#2565,#2566,#2567,#2568,#2569,#2570,#2571,#2572,
#2573,#2574,#2575,#2576,#2577,#2578,#2579,#2580,#2581,#2582));
#2691=CLOSED_SHELL('',(#2583,#2584,#2585,#2586,#2587,#2588,#2589,#2590,
#2591,#2592,#2593,#2594,#2595,#2596,#2597,#2598,#2599,#2600,#2601,#2602));
#2692=CLOSED_SHELL('',(#2603,#2604,#2605,#2606,#2607,#2608));
#2693=CLOSED_SHELL('',(#2609,#2610,#2611,#2612,#2613,#2614,#2615,#2616,
#2617,#2618,#2619));
#2694=CLOSED_SHELL('',(#2620,#2621,#2622,#2623,#2624,#2625,#2626,#2627,
#2628,#2629,#2630,#2631,#2632,#2633,#2634,#2635,#2636,#2637,#2638,#2639,
#2640,#2641,#2642,#2643,#2644,#2645,#2646,#2647,#2648,#2649,#2650,#2651,
#2652,#2653,#2654,#2655,#2656,#2657,#2658));
#2695=CLOSED_SHELL('',(#2659,#2660,#2661,#2662,#2663,#2664,#2665,#2666,
#2667,#2668,#2669,#2670));
#2696=CLOSED_SHELL('',(#2671,#2672,#2673,#2674,#2675,#2676));
#2697=CLOSED_SHELL('',(#2677,#2678,#2679,#2680,#2681,#2682,#2683,#2684,
#2685,#2686));
#2698=DERIVED_UNIT_ELEMENT(#2720,1.);
#2699=DERIVED_UNIT_ELEMENT(#4835,-3.);
#2700=DERIVED_UNIT_ELEMENT(#2720,1.);
#2701=DERIVED_UNIT_ELEMENT(#4835,-3.);
#2702=DERIVED_UNIT_ELEMENT(#2720,1.);
#2703=DERIVED_UNIT_ELEMENT(#4835,-3.);
#2704=DERIVED_UNIT_ELEMENT(#2720,1.);
#2705=DERIVED_UNIT_ELEMENT(#4835,-3.);
#2706=DERIVED_UNIT_ELEMENT(#2720,1.);
#2707=DERIVED_UNIT_ELEMENT(#4835,-3.);
#2708=DERIVED_UNIT_ELEMENT(#2720,1.);
#2709=DERIVED_UNIT_ELEMENT(#4835,-3.);
#2710=DERIVED_UNIT_ELEMENT(#2720,1.);
#2711=DERIVED_UNIT_ELEMENT(#4835,-3.);
#2712=DERIVED_UNIT_ELEMENT(#2720,1.);
#2713=DERIVED_UNIT_ELEMENT(#4835,-3.);
#2714=DERIVED_UNIT_ELEMENT(#2720,1.);
#2715=DERIVED_UNIT_ELEMENT(#4835,-3.);
#2716=DERIVED_UNIT_ELEMENT(#2720,1.);
#2717=DERIVED_UNIT_ELEMENT(#4835,-3.);
#2718=DERIVED_UNIT_ELEMENT(#2720,1.);
#2719=DERIVED_UNIT_ELEMENT(#4835,-3.);
#2720=(
MASS_UNIT()
NAMED_UNIT(*)
SI_UNIT(.KILO.,.GRAM.)
);
#2721=DERIVED_UNIT((#2698,#2699));
#2722=DERIVED_UNIT((#2700,#2701));
#2723=DERIVED_UNIT((#2702,#2703));
#2724=DERIVED_UNIT((#2704,#2705));
#2725=DERIVED_UNIT((#2706,#2707));
#2726=DERIVED_UNIT((#2708,#2709));
#2727=DERIVED_UNIT((#2710,#2711));
#2728=DERIVED_UNIT((#2712,#2713));
#2729=DERIVED_UNIT((#2714,#2715));
#2730=DERIVED_UNIT((#2716,#2717));
#2731=DERIVED_UNIT((#2718,#2719));
#2732=MEASURE_REPRESENTATION_ITEM('density measure',
POSITIVE_RATIO_MEASURE(7850.),#2721);
#2733=MEASURE_REPRESENTATION_ITEM('density measure',
POSITIVE_RATIO_MEASURE(7850.),#2722);
#2734=MEASURE_REPRESENTATION_ITEM('density measure',
POSITIVE_RATIO_MEASURE(7850.),#2723);
#2735=MEASURE_REPRESENTATION_ITEM('density measure',
POSITIVE_RATIO_MEASURE(7850.),#2724);
#2736=MEASURE_REPRESENTATION_ITEM('density measure',
POSITIVE_RATIO_MEASURE(7850.),#2725);
#2737=MEASURE_REPRESENTATION_ITEM('density measure',
POSITIVE_RATIO_MEASURE(7850.),#2726);
#2738=MEASURE_REPRESENTATION_ITEM('density measure',
POSITIVE_RATIO_MEASURE(7850.),#2727);
#2739=MEASURE_REPRESENTATION_ITEM('density measure',
POSITIVE_RATIO_MEASURE(7850.),#2728);
#2740=MEASURE_REPRESENTATION_ITEM('density measure',
POSITIVE_RATIO_MEASURE(7850.),#2729);
#2741=MEASURE_REPRESENTATION_ITEM('density measure',
POSITIVE_RATIO_MEASURE(7850.),#2730);
#2742=MEASURE_REPRESENTATION_ITEM('density measure',
POSITIVE_RATIO_MEASURE(7850.),#2731);
#2743=PROPERTY_DEFINITION_REPRESENTATION(#2798,#2765);
#2744=PROPERTY_DEFINITION_REPRESENTATION(#2799,#2766);
#2745=PROPERTY_DEFINITION_REPRESENTATION(#2800,#2767);
#2746=PROPERTY_DEFINITION_REPRESENTATION(#2801,#2768);
#2747=PROPERTY_DEFINITION_REPRESENTATION(#2802,#2769);
#2748=PROPERTY_DEFINITION_REPRESENTATION(#2803,#2770);
#2749=PROPERTY_DEFINITION_REPRESENTATION(#2804,#2771);
#2750=PROPERTY_DEFINITION_REPRESENTATION(#2805,#2772);
#2751=PROPERTY_DEFINITION_REPRESENTATION(#2806,#2773);
#2752=PROPERTY_DEFINITION_REPRESENTATION(#2807,#2774);
#2753=PROPERTY_DEFINITION_REPRESENTATION(#2808,#2775);
#2754=PROPERTY_DEFINITION_REPRESENTATION(#2809,#2776);
#2755=PROPERTY_DEFINITION_REPRESENTATION(#2810,#2777);
#2756=PROPERTY_DEFINITION_REPRESENTATION(#2811,#2778);
#2757=PROPERTY_DEFINITION_REPRESENTATION(#2812,#2779);
#2758=PROPERTY_DEFINITION_REPRESENTATION(#2813,#2780);
#2759=PROPERTY_DEFINITION_REPRESENTATION(#2814,#2781);
#2760=PROPERTY_DEFINITION_REPRESENTATION(#2815,#2782);
#2761=PROPERTY_DEFINITION_REPRESENTATION(#2816,#2783);
#2762=PROPERTY_DEFINITION_REPRESENTATION(#2817,#2784);
#2763=PROPERTY_DEFINITION_REPRESENTATION(#2818,#2785);
#2764=PROPERTY_DEFINITION_REPRESENTATION(#2819,#2786);
#2765=REPRESENTATION('material name',(#2787),#4822);
#2766=REPRESENTATION('density',(#2732),#4822);
#2767=REPRESENTATION('material name',(#2788),#4823);
#2768=REPRESENTATION('density',(#2733),#4823);
#2769=REPRESENTATION('material name',(#2789),#4824);
#2770=REPRESENTATION('density',(#2734),#4824);
#2771=REPRESENTATION('material name',(#2790),#4825);
#2772=REPRESENTATION('density',(#2735),#4825);
#2773=REPRESENTATION('material name',(#2791),#4826);
#2774=REPRESENTATION('density',(#2736),#4826);
#2775=REPRESENTATION('material name',(#2792),#4827);
#2776=REPRESENTATION('density',(#2737),#4827);
#2777=REPRESENTATION('material name',(#2793),#4828);
#2778=REPRESENTATION('density',(#2738),#4828);
#2779=REPRESENTATION('material name',(#2794),#4829);
#2780=REPRESENTATION('density',(#2739),#4829);
#2781=REPRESENTATION('material name',(#2795),#4830);
#2782=REPRESENTATION('density',(#2740),#4830);
#2783=REPRESENTATION('material name',(#2796),#4831);
#2784=REPRESENTATION('density',(#2741),#4831);
#2785=REPRESENTATION('material name',(#2797),#4832);
#2786=REPRESENTATION('density',(#2742),#4832);
#2787=DESCRIPTIVE_REPRESENTATION_ITEM('Steel','Steel');
#2788=DESCRIPTIVE_REPRESENTATION_ITEM('Steel','Steel');
#2789=DESCRIPTIVE_REPRESENTATION_ITEM('Steel','Steel');
#2790=DESCRIPTIVE_REPRESENTATION_ITEM('Steel','Steel');
#2791=DESCRIPTIVE_REPRESENTATION_ITEM('Steel','Steel');
#2792=DESCRIPTIVE_REPRESENTATION_ITEM('Steel','Steel');
#2793=DESCRIPTIVE_REPRESENTATION_ITEM('Steel','Steel');
#2794=DESCRIPTIVE_REPRESENTATION_ITEM('Steel','Steel');
#2795=DESCRIPTIVE_REPRESENTATION_ITEM('Steel','Steel');
#2796=DESCRIPTIVE_REPRESENTATION_ITEM('Steel','Steel');
#2797=DESCRIPTIVE_REPRESENTATION_ITEM('Steel','Steel');
#2798=PROPERTY_DEFINITION('material property','material name',#4887);
#2799=PROPERTY_DEFINITION('material property','density of part',#4887);
#2800=PROPERTY_DEFINITION('material property','material name',#4888);
#2801=PROPERTY_DEFINITION('material property','density of part',#4888);
#2802=PROPERTY_DEFINITION('material property','material name',#4889);
#2803=PROPERTY_DEFINITION('material property','density of part',#4889);
#2804=PROPERTY_DEFINITION('material property','material name',#4890);
#2805=PROPERTY_DEFINITION('material property','density of part',#4890);
#2806=PROPERTY_DEFINITION('material property','material name',#4891);
#2807=PROPERTY_DEFINITION('material property','density of part',#4891);
#2808=PROPERTY_DEFINITION('material property','material name',#4892);
#2809=PROPERTY_DEFINITION('material property','density of part',#4892);
#2810=PROPERTY_DEFINITION('material property','material name',#4893);
#2811=PROPERTY_DEFINITION('material property','density of part',#4893);
#2812=PROPERTY_DEFINITION('material property','material name',#4894);
#2813=PROPERTY_DEFINITION('material property','density of part',#4894);
#2814=PROPERTY_DEFINITION('material property','material name',#4895);
#2815=PROPERTY_DEFINITION('material property','density of part',#4895);
#2816=PROPERTY_DEFINITION('material property','material name',#4896);
#2817=PROPERTY_DEFINITION('material property','density of part',#4896);
#2818=PROPERTY_DEFINITION('material property','material name',#4897);
#2819=PROPERTY_DEFINITION('material property','density of part',#4897);
#2820=AXIS2_PLACEMENT_3D('',#3884,#3090,#3091);
#2821=AXIS2_PLACEMENT_3D('',#3885,#3092,#3093);
#2822=AXIS2_PLACEMENT_3D('',#3886,#3094,#3095);
#2823=AXIS2_PLACEMENT_3D('',#3888,#3096,#3097);
#2824=AXIS2_PLACEMENT_3D('',#3891,#3099,#3100);
#2825=AXIS2_PLACEMENT_3D('',#3892,#3101,#3102);
#2826=AXIS2_PLACEMENT_3D('',#3893,#3103,#3104);
#2827=AXIS2_PLACEMENT_3D('',#3895,#3105,#3106);
#2828=AXIS2_PLACEMENT_3D('',#3898,#3108,#3109);
#2829=AXIS2_PLACEMENT_3D('',#3899,#3110,#3111);
#2830=AXIS2_PLACEMENT_3D('',#3900,#3112,#3113);
#2831=AXIS2_PLACEMENT_3D('',#3902,#3114,#3115);
#2832=AXIS2_PLACEMENT_3D('',#3905,#3117,#3118);
#2833=AXIS2_PLACEMENT_3D('',#3906,#3119,#3120);
#2834=AXIS2_PLACEMENT_3D('',#3907,#3121,#3122);
#2835=AXIS2_PLACEMENT_3D('',#3909,#3123,#3124);
#2836=AXIS2_PLACEMENT_3D('',#3912,#3126,#3127);
#2837=AXIS2_PLACEMENT_3D('',#3913,#3128,#3129);
#2838=AXIS2_PLACEMENT_3D('',#3914,#3130,#3131);
#2839=AXIS2_PLACEMENT_3D('',#3916,#3132,#3133);
#2840=AXIS2_PLACEMENT_3D('',#3919,#3135,#3136);
#2841=AXIS2_PLACEMENT_3D('',#3920,#3137,#3138);
#2842=AXIS2_PLACEMENT_3D('',#3921,#3139,#3140);
#2843=AXIS2_PLACEMENT_3D('',#3923,#3141,#3142);
#2844=AXIS2_PLACEMENT_3D('',#3926,#3144,#3145);
#2845=AXIS2_PLACEMENT_3D('',#3927,#3146,#3147);
#2846=AXIS2_PLACEMENT_3D('',#3928,#3148,#3149);
#2847=AXIS2_PLACEMENT_3D('',#3937,#3154,#3155);
#2848=AXIS2_PLACEMENT_3D('',#3943,#3159,#3160);
#2849=AXIS2_PLACEMENT_3D('',#3949,#3164,#3165);
#2850=AXIS2_PLACEMENT_3D('',#3952,#3168,#3169);
#2851=AXIS2_PLACEMENT_3D('',#3953,#3170,#3171);
#2852=AXIS2_PLACEMENT_3D('',#3954,#3172,#3173);
#2853=AXIS2_PLACEMENT_3D('',#3955,#3174,#3175);
#2854=AXIS2_PLACEMENT_3D('',#3957,#3176,#3177);
#2855=AXIS2_PLACEMENT_3D('',#3960,#3179,#3180);
#2856=AXIS2_PLACEMENT_3D('',#3961,#3181,#3182);
#2857=AXIS2_PLACEMENT_3D('',#3962,#3183,#3184);
#2858=AXIS2_PLACEMENT_3D('',#3964,#3185,#3186);
#2859=AXIS2_PLACEMENT_3D('',#3967,#3188,#3189);
#2860=AXIS2_PLACEMENT_3D('',#3968,#3190,#3191);
#2861=AXIS2_PLACEMENT_3D('',#3969,#3192,#3193);
#2862=AXIS2_PLACEMENT_3D('',#3971,#3194,#3195);
#2863=AXIS2_PLACEMENT_3D('',#3974,#3197,#3198);
#2864=AXIS2_PLACEMENT_3D('',#3975,#3199,#3200);
#2865=AXIS2_PLACEMENT_3D('',#3976,#3201,#3202);
#2866=AXIS2_PLACEMENT_3D('',#3978,#3203,#3204);
#2867=AXIS2_PLACEMENT_3D('',#3981,#3206,#3207);
#2868=AXIS2_PLACEMENT_3D('',#3982,#3208,#3209);
#2869=AXIS2_PLACEMENT_3D('',#3983,#3210,#3211);
#2870=AXIS2_PLACEMENT_3D('',#3985,#3212,#3213);
#2871=AXIS2_PLACEMENT_3D('',#3988,#3215,#3216);
#2872=AXIS2_PLACEMENT_3D('',#3989,#3217,#3218);
#2873=AXIS2_PLACEMENT_3D('',#3990,#3219,#3220);
#2874=AXIS2_PLACEMENT_3D('',#3992,#3221,#3222);
#2875=AXIS2_PLACEMENT_3D('',#3995,#3224,#3225);
#2876=AXIS2_PLACEMENT_3D('',#3996,#3226,#3227);
#2877=AXIS2_PLACEMENT_3D('',#3997,#3228,#3229);
#2878=AXIS2_PLACEMENT_3D('',#4006,#3234,#3235);
#2879=AXIS2_PLACEMENT_3D('',#4012,#3239,#3240);
#2880=AXIS2_PLACEMENT_3D('',#4018,#3244,#3245);
#2881=AXIS2_PLACEMENT_3D('',#4021,#3248,#3249);
#2882=AXIS2_PLACEMENT_3D('',#4022,#3250,#3251);
#2883=AXIS2_PLACEMENT_3D('',#4023,#3252,#3253);
#2884=AXIS2_PLACEMENT_3D('',#4024,#3254,#3255);
#2885=AXIS2_PLACEMENT_3D('',#4026,#3256,#3257);
#2886=AXIS2_PLACEMENT_3D('',#4029,#3259,#3260);
#2887=AXIS2_PLACEMENT_3D('',#4030,#3261,#3262);
#2888=AXIS2_PLACEMENT_3D('',#4031,#3263,#3264);
#2889=AXIS2_PLACEMENT_3D('',#4032,#3265,#3266);
#2890=AXIS2_PLACEMENT_3D('',#4033,#3267,#3268);
#2891=AXIS2_PLACEMENT_3D('',#4038,#3270,#3271);
#2892=AXIS2_PLACEMENT_3D('',#4041,#3273,#3274);
#2893=AXIS2_PLACEMENT_3D('',#4042,#3275,#3276);
#2894=AXIS2_PLACEMENT_3D('',#4046,#3278,#3279);
#2895=AXIS2_PLACEMENT_3D('',#4048,#3281,#3282);
#2896=AXIS2_PLACEMENT_3D('',#4052,#3284,#3285);
#2897=AXIS2_PLACEMENT_3D('',#4054,#3287,#3288);
#2898=AXIS2_PLACEMENT_3D('',#4059,#3290,#3291);
#2899=AXIS2_PLACEMENT_3D('',#4062,#3293,#3294);
#2900=AXIS2_PLACEMENT_3D('',#4063,#3295,#3296);
#2901=AXIS2_PLACEMENT_3D('',#4068,#3299,#3300);
#2902=AXIS2_PLACEMENT_3D('',#4069,#3301,#3302);
#2903=AXIS2_PLACEMENT_3D('',#4072,#3305,#3306);
#2904=AXIS2_PLACEMENT_3D('',#4077,#3309,#3310);
#2905=AXIS2_PLACEMENT_3D('',#4078,#3311,#3312);
#2906=AXIS2_PLACEMENT_3D('',#4081,#3315,#3316);
#2907=AXIS2_PLACEMENT_3D('',#4087,#3320,#3321);
#2908=AXIS2_PLACEMENT_3D('',#4091,#3324,#3325);
#2909=AXIS2_PLACEMENT_3D('',#4095,#3328,#3329);
#2910=AXIS2_PLACEMENT_3D('',#4099,#3332,#3333);
#2911=AXIS2_PLACEMENT_3D('',#4100,#3334,#3335);
#2912=AXIS2_PLACEMENT_3D('',#4106,#3339,#3340);
#2913=AXIS2_PLACEMENT_3D('',#4108,#3342,#3343);
#2914=AXIS2_PLACEMENT_3D('',#4112,#3346,#3347);
#2915=AXIS2_PLACEMENT_3D('',#4114,#3349,#3350);
#2916=AXIS2_PLACEMENT_3D('',#4115,#3351,#3352);
#2917=AXIS2_PLACEMENT_3D('',#4116,#3353,#3354);
#2918=AXIS2_PLACEMENT_3D('',#4121,#3356,#3357);
#2919=AXIS2_PLACEMENT_3D('',#4124,#3359,#3360);
#2920=AXIS2_PLACEMENT_3D('',#4125,#3361,#3362);
#2921=AXIS2_PLACEMENT_3D('',#4129,#3364,#3365);
#2922=AXIS2_PLACEMENT_3D('',#4131,#3367,#3368);
#2923=AXIS2_PLACEMENT_3D('',#4136,#3370,#3371);
#2924=AXIS2_PLACEMENT_3D('',#4139,#3373,#3374);
#2925=AXIS2_PLACEMENT_3D('',#4140,#3375,#3376);
#2926=AXIS2_PLACEMENT_3D('',#4143,#3379,#3380);
#2927=AXIS2_PLACEMENT_3D('',#4148,#3383,#3384);
#2928=AXIS2_PLACEMENT_3D('',#4149,#3385,#3386);
#2929=AXIS2_PLACEMENT_3D('',#4154,#3389,#3390);
#2930=AXIS2_PLACEMENT_3D('',#4155,#3391,#3392);
#2931=AXIS2_PLACEMENT_3D('',#4160,#3395,#3396);
#2932=AXIS2_PLACEMENT_3D('',#4161,#3397,#3398);
#2933=AXIS2_PLACEMENT_3D('',#4164,#3401,#3402);
#2934=AXIS2_PLACEMENT_3D('',#4170,#3406,#3407);
#2935=AXIS2_PLACEMENT_3D('',#4178,#3412,#3413);
#2936=AXIS2_PLACEMENT_3D('',#4182,#3416,#3417);
#2937=AXIS2_PLACEMENT_3D('',#4186,#3420,#3421);
#2938=AXIS2_PLACEMENT_3D('',#4187,#3422,#3423);
#2939=AXIS2_PLACEMENT_3D('',#4193,#3427,#3428);
#2940=AXIS2_PLACEMENT_3D('',#4197,#3431,#3432);
#2941=AXIS2_PLACEMENT_3D('',#4199,#3434,#3435);
#2942=AXIS2_PLACEMENT_3D('',#4203,#3438,#3439);
#2943=AXIS2_PLACEMENT_3D('',#4207,#3442,#3443);
#2944=AXIS2_PLACEMENT_3D('',#4209,#3445,#3446);
#2945=AXIS2_PLACEMENT_3D('',#4210,#3447,#3448);
#2946=AXIS2_PLACEMENT_3D('',#4211,#3449,#3450);
#2947=AXIS2_PLACEMENT_3D('',#4213,#3451,#3452);
#2948=AXIS2_PLACEMENT_3D('',#4216,#3454,#3455);
#2949=AXIS2_PLACEMENT_3D('',#4217,#3456,#3457);
#2950=AXIS2_PLACEMENT_3D('',#4219,#3458,#3459);
#2951=AXIS2_PLACEMENT_3D('',#4222,#3461,#3462);
#2952=AXIS2_PLACEMENT_3D('',#4223,#3463,#3464);
#2953=AXIS2_PLACEMENT_3D('',#4224,#3465,#3466);
#2954=AXIS2_PLACEMENT_3D('',#4226,#3467,#3468);
#2955=AXIS2_PLACEMENT_3D('',#4229,#3470,#3471);
#2956=AXIS2_PLACEMENT_3D('',#4230,#3472,#3473);
#2957=AXIS2_PLACEMENT_3D('',#4231,#3474,#3475);
#2958=AXIS2_PLACEMENT_3D('',#4232,#3476,#3477);
#2959=AXIS2_PLACEMENT_3D('',#4233,#3478,#3479);
#2960=AXIS2_PLACEMENT_3D('',#4242,#3484,#3485);
#2961=AXIS2_PLACEMENT_3D('',#4248,#3489,#3490);
#2962=AXIS2_PLACEMENT_3D('',#4254,#3494,#3495);
#2963=AXIS2_PLACEMENT_3D('',#4260,#3499,#3500);
#2964=AXIS2_PLACEMENT_3D('',#4266,#3504,#3505);
#2965=AXIS2_PLACEMENT_3D('',#4272,#3509,#3510);
#2966=AXIS2_PLACEMENT_3D('',#4278,#3514,#3515);
#2967=AXIS2_PLACEMENT_3D('',#4284,#3519,#3520);
#2968=AXIS2_PLACEMENT_3D('',#4287,#3523,#3524);
#2969=AXIS2_PLACEMENT_3D('',#4288,#3525,#3526);
#2970=AXIS2_PLACEMENT_3D('',#4289,#3527,#3528);
#2971=AXIS2_PLACEMENT_3D('',#4290,#3529,#3530);
#2972=AXIS2_PLACEMENT_3D('',#4292,#3531,#3532);
#2973=AXIS2_PLACEMENT_3D('',#4340,#3534,#3535);
#2974=AXIS2_PLACEMENT_3D('',#4389,#3537,#3538);
#2975=AXIS2_PLACEMENT_3D('',#4390,#3539,#3540);
#2976=AXIS2_PLACEMENT_3D('',#4392,#3541,#3542);
#2977=AXIS2_PLACEMENT_3D('',#4395,#3544,#3545);
#2978=AXIS2_PLACEMENT_3D('',#4396,#3546,#3547);
#2979=AXIS2_PLACEMENT_3D('',#4398,#3548,#3549);
#2980=AXIS2_PLACEMENT_3D('',#4401,#3551,#3552);
#2981=AXIS2_PLACEMENT_3D('',#4402,#3553,#3554);
#2982=AXIS2_PLACEMENT_3D('',#4404,#3555,#3556);
#2983=AXIS2_PLACEMENT_3D('',#4452,#3558,#3559);
#2984=AXIS2_PLACEMENT_3D('',#4501,#3561,#3562);
#2985=AXIS2_PLACEMENT_3D('',#4502,#3563,#3564);
#2986=AXIS2_PLACEMENT_3D('',#4504,#3565,#3566);
#2987=AXIS2_PLACEMENT_3D('',#4507,#3568,#3569);
#2988=AXIS2_PLACEMENT_3D('',#4508,#3570,#3571);
#2989=AXIS2_PLACEMENT_3D('',#4510,#3572,#3573);
#2990=AXIS2_PLACEMENT_3D('',#4513,#3575,#3576);
#2991=AXIS2_PLACEMENT_3D('',#4514,#3577,#3578);
#2992=AXIS2_PLACEMENT_3D('',#4517,#3579,#3580);
#2993=AXIS2_PLACEMENT_3D('',#4519,#3581,#3582);
#2994=AXIS2_PLACEMENT_3D('',#4520,#3583,#3584);
#2995=AXIS2_PLACEMENT_3D('',#4521,#3585,#3586);
#2996=AXIS2_PLACEMENT_3D('',#4524,#3587,#3588);
#2997=AXIS2_PLACEMENT_3D('',#4527,#3591,#3592);
#2998=AXIS2_PLACEMENT_3D('',#4530,#3593,#3594);
#2999=AXIS2_PLACEMENT_3D('',#4532,#3595,#3596);
#3000=AXIS2_PLACEMENT_3D('',#4533,#3597,#3598);
#3001=AXIS2_PLACEMENT_3D('',#4534,#3599,#3600);
#3002=AXIS2_PLACEMENT_3D('',#4537,#3601,#3602);
#3003=AXIS2_PLACEMENT_3D('',#4540,#3605,#3606);
#3004=AXIS2_PLACEMENT_3D('',#4543,#3607,#3608);
#3005=AXIS2_PLACEMENT_3D('',#4545,#3609,#3610);
#3006=AXIS2_PLACEMENT_3D('',#4546,#3611,#3612);
#3007=AXIS2_PLACEMENT_3D('',#4547,#3613,#3614);
#3008=AXIS2_PLACEMENT_3D('',#4550,#3615,#3616);
#3009=AXIS2_PLACEMENT_3D('',#4553,#3619,#3620);
#3010=AXIS2_PLACEMENT_3D('',#4556,#3623,#3624);
#3011=AXIS2_PLACEMENT_3D('',#4559,#3625,#3626);
#3012=AXIS2_PLACEMENT_3D('',#4561,#3627,#3628);
#3013=AXIS2_PLACEMENT_3D('',#4562,#3629,#3630);
#3014=AXIS2_PLACEMENT_3D('',#4563,#3631,#3632);
#3015=AXIS2_PLACEMENT_3D('',#4566,#3633,#3634);
#3016=AXIS2_PLACEMENT_3D('',#4569,#3637,#3638);
#3017=AXIS2_PLACEMENT_3D('',#4572,#3641,#3642);
#3018=AXIS2_PLACEMENT_3D('',#4575,#3645,#3646);
#3019=AXIS2_PLACEMENT_3D('',#4578,#3649,#3650);
#3020=AXIS2_PLACEMENT_3D('',#4605,#3664,#3665);
#3021=AXIS2_PLACEMENT_3D('',#4606,#3666,#3667);
#3022=AXIS2_PLACEMENT_3D('',#4608,#3669,#3670);
#3023=AXIS2_PLACEMENT_3D('',#4612,#3673,#3674);
#3024=AXIS2_PLACEMENT_3D('',#4613,#3675,#3676);
#3025=AXIS2_PLACEMENT_3D('',#4616,#3678,#3679);
#3026=AXIS2_PLACEMENT_3D('',#4617,#3680,#3681);
#3027=AXIS2_PLACEMENT_3D('',#4623,#3685,#3686);
#3028=AXIS2_PLACEMENT_3D('',#4629,#3690,#3691);
#3029=AXIS2_PLACEMENT_3D('',#4631,#3693,#3694);
#3030=AXIS2_PLACEMENT_3D('',#4635,#3697,#3698);
#3031=AXIS2_PLACEMENT_3D('',#4641,#3702,#3703);
#3032=AXIS2_PLACEMENT_3D('',#4643,#3705,#3706);
#3033=AXIS2_PLACEMENT_3D('',#4646,#3709,#3710);
#3034=AXIS2_PLACEMENT_3D('',#4650,#3713,#3714);
#3035=AXIS2_PLACEMENT_3D('',#4654,#3717,#3718);
#3036=AXIS2_PLACEMENT_3D('',#4658,#3721,#3722);
#3037=AXIS2_PLACEMENT_3D('',#4662,#3725,#3726);
#3038=AXIS2_PLACEMENT_3D('',#4664,#3728,#3729);
#3039=AXIS2_PLACEMENT_3D('',#4665,#3730,#3731);
#3040=AXIS2_PLACEMENT_3D('',#4666,#3732,#3733);
#3041=AXIS2_PLACEMENT_3D('',#4667,#3734,#3735);
#3042=AXIS2_PLACEMENT_3D('',#4669,#3736,#3737);
#3043=AXIS2_PLACEMENT_3D('',#4672,#3739,#3740);
#3044=AXIS2_PLACEMENT_3D('',#4673,#3741,#3742);
#3045=AXIS2_PLACEMENT_3D('',#4674,#3743,#3744);
#3046=AXIS2_PLACEMENT_3D('',#4683,#3749,#3750);
#3047=AXIS2_PLACEMENT_3D('',#4697,#3758,#3759);
#3048=AXIS2_PLACEMENT_3D('',#4701,#3762,#3763);
#3049=AXIS2_PLACEMENT_3D('',#4705,#3766,#3767);
#3050=AXIS2_PLACEMENT_3D('',#4711,#3771,#3772);
#3051=AXIS2_PLACEMENT_3D('',#4715,#3775,#3776);
#3052=AXIS2_PLACEMENT_3D('',#4719,#3779,#3780);
#3053=AXIS2_PLACEMENT_3D('',#4721,#3782,#3783);
#3054=AXIS2_PLACEMENT_3D('',#4723,#3785,#3786);
#3055=AXIS2_PLACEMENT_3D('',#4724,#3787,#3788);
#3056=AXIS2_PLACEMENT_3D('',#4725,#3789,#3790);
#3057=AXIS2_PLACEMENT_3D('',#4727,#3791,#3792);
#3058=AXIS2_PLACEMENT_3D('',#4730,#3794,#3795);
#3059=AXIS2_PLACEMENT_3D('',#4731,#3796,#3797);
#3060=AXIS2_PLACEMENT_3D('',#4733,#3798,#3799);
#3061=AXIS2_PLACEMENT_3D('',#4736,#3801,#3802);
#3062=AXIS2_PLACEMENT_3D('',#4737,#3803,#3804);
#3063=AXIS2_PLACEMENT_3D('',#4738,#3805,#3806);
#3064=AXIS2_PLACEMENT_3D('',#4740,#3807,#3808);
#3065=AXIS2_PLACEMENT_3D('',#4743,#3810,#3811);
#3066=AXIS2_PLACEMENT_3D('',#4744,#3812,#3813);
#3067=AXIS2_PLACEMENT_3D('',#4745,#3814,#3815);
#3068=AXIS2_PLACEMENT_3D('',#4746,#3816,#3817);
#3069=AXIS2_PLACEMENT_3D('',#4747,#3818,#3819);
#3070=AXIS2_PLACEMENT_3D('',#4756,#3824,#3825);
#3071=AXIS2_PLACEMENT_3D('',#4762,#3829,#3830);
#3072=AXIS2_PLACEMENT_3D('',#4774,#3837,#3838);
#3073=AXIS2_PLACEMENT_3D('',#4778,#3841,#3842);
#3074=AXIS2_PLACEMENT_3D('',#4782,#3845,#3846);
#3075=AXIS2_PLACEMENT_3D('',#4788,#3850,#3851);
#3076=AXIS2_PLACEMENT_3D('',#4790,#3853,#3854);
#3077=AXIS2_PLACEMENT_3D('',#4794,#3857,#3858);
#3078=AXIS2_PLACEMENT_3D('',#4796,#3860,#3861);
#3079=AXIS2_PLACEMENT_3D('',#4797,#3862,#3863);
#3080=AXIS2_PLACEMENT_3D('',#4798,#3864,#3865);
#3081=AXIS2_PLACEMENT_3D('',#4799,#3866,#3867);
#3082=AXIS2_PLACEMENT_3D('',#4800,#3868,#3869);
#3083=AXIS2_PLACEMENT_3D('',#4801,#3870,#3871);
#3084=AXIS2_PLACEMENT_3D('',#4802,#3872,#3873);
#3085=AXIS2_PLACEMENT_3D('',#4803,#3874,#3875);
#3086=AXIS2_PLACEMENT_3D('',#4804,#3876,#3877);
#3087=AXIS2_PLACEMENT_3D('',#4805,#3878,#3879);
#3088=AXIS2_PLACEMENT_3D('',#4806,#3880,#3881);
#3089=AXIS2_PLACEMENT_3D('',#4807,#3882,#3883);
#3090=DIRECTION('axis',(0.,0.,1.));
#3091=DIRECTION('refdir',(1.,0.,0.));
#3092=DIRECTION('axis',(0.,0.,1.));
#3093=DIRECTION('refdir',(1.,0.,0.));
#3094=DIRECTION('center_axis',(0.,0.,-1.));
#3095=DIRECTION('ref_axis',(-1.,0.,0.));
#3096=DIRECTION('center_axis',(0.,0.,-1.));
#3097=DIRECTION('ref_axis',(-1.,0.,0.));
#3098=DIRECTION('',(0.,0.,-1.));
#3099=DIRECTION('center_axis',(0.,0.,-1.));
#3100=DIRECTION('ref_axis',(-1.,0.,0.));
#3101=DIRECTION('center_axis',(0.,0.,1.));
#3102=DIRECTION('ref_axis',(-1.,0.,0.));
#3103=DIRECTION('center_axis',(0.,0.,-1.));
#3104=DIRECTION('ref_axis',(-1.,0.,0.));
#3105=DIRECTION('center_axis',(0.,0.,-1.));
#3106=DIRECTION('ref_axis',(-1.,0.,0.));
#3107=DIRECTION('',(0.,0.,-1.));
#3108=DIRECTION('center_axis',(0.,0.,-1.));
#3109=DIRECTION('ref_axis',(-1.,0.,0.));
#3110=DIRECTION('center_axis',(0.,0.,1.));
#3111=DIRECTION('ref_axis',(-1.,0.,0.));
#3112=DIRECTION('center_axis',(0.,0.,-1.));
#3113=DIRECTION('ref_axis',(-1.,0.,0.));
#3114=DIRECTION('center_axis',(0.,0.,-1.));
#3115=DIRECTION('ref_axis',(-1.,0.,0.));
#3116=DIRECTION('',(0.,0.,-1.));
#3117=DIRECTION('center_axis',(0.,0.,-1.));
#3118=DIRECTION('ref_axis',(-1.,0.,0.));
#3119=DIRECTION('center_axis',(0.,0.,1.));
#3120=DIRECTION('ref_axis',(-1.,0.,0.));
#3121=DIRECTION('center_axis',(0.,0.,-1.));
#3122=DIRECTION('ref_axis',(-1.,0.,0.));
#3123=DIRECTION('center_axis',(0.,0.,-1.));
#3124=DIRECTION('ref_axis',(-1.,0.,0.));
#3125=DIRECTION('',(0.,0.,-1.));
#3126=DIRECTION('center_axis',(0.,0.,-1.));
#3127=DIRECTION('ref_axis',(-1.,0.,0.));
#3128=DIRECTION('center_axis',(0.,0.,1.));
#3129=DIRECTION('ref_axis',(-1.,0.,0.));
#3130=DIRECTION('center_axis',(0.,0.,-1.));
#3131=DIRECTION('ref_axis',(-1.,0.,0.));
#3132=DIRECTION('center_axis',(0.,0.,-1.));
#3133=DIRECTION('ref_axis',(-1.,0.,0.));
#3134=DIRECTION('',(0.,0.,-1.));
#3135=DIRECTION('center_axis',(0.,0.,-1.));
#3136=DIRECTION('ref_axis',(-1.,0.,0.));
#3137=DIRECTION('center_axis',(0.,0.,1.));
#3138=DIRECTION('ref_axis',(-1.,0.,0.));
#3139=DIRECTION('center_axis',(0.,0.,-1.));
#3140=DIRECTION('ref_axis',(-1.,0.,0.));
#3141=DIRECTION('center_axis',(0.,0.,-1.));
#3142=DIRECTION('ref_axis',(-1.,0.,0.));
#3143=DIRECTION('',(0.,0.,-1.));
#3144=DIRECTION('center_axis',(0.,0.,-1.));
#3145=DIRECTION('ref_axis',(-1.,0.,0.));
#3146=DIRECTION('center_axis',(0.,0.,1.));
#3147=DIRECTION('ref_axis',(-1.,0.,0.));
#3148=DIRECTION('center_axis',(1.,0.,0.));
#3149=DIRECTION('ref_axis',(0.,1.,0.));
#3150=DIRECTION('',(0.,1.,0.));
#3151=DIRECTION('',(0.,0.,1.));
#3152=DIRECTION('',(0.,1.,0.));
#3153=DIRECTION('',(0.,0.,1.));
#3154=DIRECTION('center_axis',(0.,-1.,0.));
#3155=DIRECTION('ref_axis',(1.,0.,0.));
#3156=DIRECTION('',(1.,0.,0.));
#3157=DIRECTION('',(1.,0.,0.));
#3158=DIRECTION('',(0.,0.,1.));
#3159=DIRECTION('center_axis',(-1.,0.,0.));
#3160=DIRECTION('ref_axis',(0.,-1.,0.));
#3161=DIRECTION('',(0.,-1.,0.));
#3162=DIRECTION('',(0.,-1.,0.));
#3163=DIRECTION('',(0.,0.,1.));
#3164=DIRECTION('center_axis',(0.,1.,0.));
#3165=DIRECTION('ref_axis',(-1.,0.,0.));
#3166=DIRECTION('',(-1.,0.,0.));
#3167=DIRECTION('',(-1.,0.,0.));
#3168=DIRECTION('center_axis',(0.,0.,1.));
#3169=DIRECTION('ref_axis',(1.,0.,0.));
#3170=DIRECTION('center_axis',(0.,0.,1.));
#3171=DIRECTION('ref_axis',(-1.,0.,0.));
#3172=DIRECTION('axis',(0.,0.,1.));
#3173=DIRECTION('refdir',(1.,0.,0.));
#3174=DIRECTION('center_axis',(0.,0.,-1.));
#3175=DIRECTION('ref_axis',(-1.,0.,0.));
#3176=DIRECTION('center_axis',(0.,0.,-1.));
#3177=DIRECTION('ref_axis',(-1.,0.,0.));
#3178=DIRECTION('',(0.,0.,-1.));
#3179=DIRECTION('center_axis',(0.,0.,-1.));
#3180=DIRECTION('ref_axis',(-1.,0.,0.));
#3181=DIRECTION('center_axis',(0.,0.,1.));
#3182=DIRECTION('ref_axis',(-1.,0.,0.));
#3183=DIRECTION('center_axis',(0.,0.,-1.));
#3184=DIRECTION('ref_axis',(-1.,0.,0.));
#3185=DIRECTION('center_axis',(0.,0.,-1.));
#3186=DIRECTION('ref_axis',(-1.,0.,0.));
#3187=DIRECTION('',(0.,0.,-1.));
#3188=DIRECTION('center_axis',(0.,0.,-1.));
#3189=DIRECTION('ref_axis',(-1.,0.,0.));
#3190=DIRECTION('center_axis',(0.,0.,1.));
#3191=DIRECTION('ref_axis',(-1.,0.,0.));
#3192=DIRECTION('center_axis',(0.,0.,-1.));
#3193=DIRECTION('ref_axis',(-1.,0.,0.));
#3194=DIRECTION('center_axis',(0.,0.,-1.));
#3195=DIRECTION('ref_axis',(-1.,0.,0.));
#3196=DIRECTION('',(0.,0.,-1.));
#3197=DIRECTION('center_axis',(0.,0.,-1.));
#3198=DIRECTION('ref_axis',(-1.,0.,0.));
#3199=DIRECTION('center_axis',(0.,0.,1.));
#3200=DIRECTION('ref_axis',(-1.,0.,0.));
#3201=DIRECTION('center_axis',(0.,0.,-1.));
#3202=DIRECTION('ref_axis',(-1.,0.,0.));
#3203=DIRECTION('center_axis',(0.,0.,-1.));
#3204=DIRECTION('ref_axis',(-1.,0.,0.));
#3205=DIRECTION('',(0.,0.,-1.));
#3206=DIRECTION('center_axis',(0.,0.,-1.));
#3207=DIRECTION('ref_axis',(-1.,0.,0.));
#3208=DIRECTION('center_axis',(0.,0.,1.));
#3209=DIRECTION('ref_axis',(-1.,0.,0.));
#3210=DIRECTION('center_axis',(0.,0.,-1.));
#3211=DIRECTION('ref_axis',(-1.,0.,0.));
#3212=DIRECTION('center_axis',(0.,0.,-1.));
#3213=DIRECTION('ref_axis',(-1.,0.,0.));
#3214=DIRECTION('',(0.,0.,-1.));
#3215=DIRECTION('center_axis',(0.,0.,-1.));
#3216=DIRECTION('ref_axis',(-1.,0.,0.));
#3217=DIRECTION('center_axis',(0.,0.,1.));
#3218=DIRECTION('ref_axis',(-1.,0.,0.));
#3219=DIRECTION('center_axis',(0.,0.,-1.));
#3220=DIRECTION('ref_axis',(-1.,0.,0.));
#3221=DIRECTION('center_axis',(0.,0.,-1.));
#3222=DIRECTION('ref_axis',(-1.,0.,0.));
#3223=DIRECTION('',(0.,0.,-1.));
#3224=DIRECTION('center_axis',(0.,0.,-1.));
#3225=DIRECTION('ref_axis',(-1.,0.,0.));
#3226=DIRECTION('center_axis',(0.,0.,1.));
#3227=DIRECTION('ref_axis',(-1.,0.,0.));
#3228=DIRECTION('center_axis',(1.,0.,0.));
#3229=DIRECTION('ref_axis',(0.,1.,0.));
#3230=DIRECTION('',(0.,-1.,0.));
#3231=DIRECTION('',(0.,0.,1.));
#3232=DIRECTION('',(0.,1.,0.));
#3233=DIRECTION('',(0.,0.,1.));
#3234=DIRECTION('center_axis',(0.,-1.,0.));
#3235=DIRECTION('ref_axis',(1.,0.,0.));
#3236=DIRECTION('',(-1.,0.,0.));
#3237=DIRECTION('',(1.,0.,0.));
#3238=DIRECTION('',(0.,0.,1.));
#3239=DIRECTION('center_axis',(-1.,0.,0.));
#3240=DIRECTION('ref_axis',(0.,-1.,0.));
#3241=DIRECTION('',(0.,1.,0.));
#3242=DIRECTION('',(0.,-1.,0.));
#3243=DIRECTION('',(0.,0.,1.));
#3244=DIRECTION('center_axis',(0.,1.,0.));
#3245=DIRECTION('ref_axis',(-1.,0.,0.));
#3246=DIRECTION('',(1.,0.,0.));
#3247=DIRECTION('',(-1.,0.,0.));
#3248=DIRECTION('center_axis',(0.,0.,1.));
#3249=DIRECTION('ref_axis',(1.,0.,0.));
#3250=DIRECTION('center_axis',(0.,0.,1.));
#3251=DIRECTION('ref_axis',(-1.,0.,0.));
#3252=DIRECTION('axis',(0.,0.,1.));
#3253=DIRECTION('refdir',(1.,0.,0.));
#3254=DIRECTION('center_axis',(-1.,0.,0.));
#3255=DIRECTION('ref_axis',(0.,-1.,0.));
#3256=DIRECTION('center_axis',(-1.,0.,0.));
#3257=DIRECTION('ref_axis',(0.,-1.,0.));
#3258=DIRECTION('',(1.,0.,0.));
#3259=DIRECTION('center_axis',(-1.,0.,0.));
#3260=DIRECTION('ref_axis',(0.,-1.,0.));
#3261=DIRECTION('center_axis',(-1.,0.,0.));
#3262=DIRECTION('ref_axis',(0.,-1.,0.));
#3263=DIRECTION('center_axis',(-1.,0.,0.));
#3264=DIRECTION('ref_axis',(0.,-1.,0.));
#3265=DIRECTION('axis',(0.,0.,1.));
#3266=DIRECTION('refdir',(1.,0.,0.));
#3267=DIRECTION('center_axis',(0.,0.707106781186548,0.707106781186548));
#3268=DIRECTION('ref_axis',(-0.707106781186553,-0.499999999999996,0.499999999999996));
#3269=DIRECTION('',(0.,-0.707106781186548,-0.707106781186548));
#3270=DIRECTION('center_axis',(0.,0.382683432365092,0.923879532511286));
#3271=DIRECTION('ref_axis',(0.,-0.923879532511286,0.382683432365091));
#3272=DIRECTION('',(0.,0.707106781186548,0.707106781186548));
#3273=DIRECTION('center_axis',(-8.497279155086E-16,-0.923879532511287,-0.382683432365089));
#3274=DIRECTION('ref_axis',(2.05142465794788E-15,0.382683432365089,-0.923879532511287));
#3275=DIRECTION('center_axis',(0.,0.,-1.));
#3276=DIRECTION('ref_axis',(-0.707106781186548,-0.707106781186548,0.));
#3277=DIRECTION('',(0.,0.,-1.));
#3278=DIRECTION('center_axis',(2.05142465794792E-15,-0.382683432365088,
0.923879532511288));
#3279=DIRECTION('ref_axis',(-4.95257723140449E-15,0.923879532511288,0.382683432365088));
#3280=DIRECTION('',(0.,0.,1.));
#3281=DIRECTION('center_axis',(0.,-0.707106781186548,0.707106781186547));
#3282=DIRECTION('ref_axis',(-0.707106781186553,-0.499999999999996,-0.499999999999996));
#3283=DIRECTION('',(0.,0.707106781186548,-0.707106781186547));
#3284=DIRECTION('center_axis',(0.,-0.923879532511286,0.382683432365091));
#3285=DIRECTION('ref_axis',(0.,-0.382683432365091,-0.923879532511286));
#3286=DIRECTION('',(0.,-0.707106781186548,0.707106781186547));
#3287=DIRECTION('center_axis',(0.,-0.707106781186548,-0.707106781186548));
#3288=DIRECTION('ref_axis',(-0.707106781186553,0.499999999999996,-0.499999999999996));
#3289=DIRECTION('',(0.,0.707106781186548,0.707106781186548));
#3290=DIRECTION('center_axis',(0.,-0.382683432365093,-0.923879532511285));
#3291=DIRECTION('ref_axis',(0.,0.923879532511285,-0.382683432365093));
#3292=DIRECTION('',(0.,-0.707106781186548,-0.707106781186548));
#3293=DIRECTION('center_axis',(0.,0.923879532511287,0.38268343236509));
#3294=DIRECTION('ref_axis',(0.,-0.38268343236509,0.923879532511287));
#3295=DIRECTION('center_axis',(0.,0.,1.));
#3296=DIRECTION('ref_axis',(-0.707106781186548,0.707106781186548,0.));
#3297=DIRECTION('',(0.,0.,-1.));
#3298=DIRECTION('',(0.,0.,1.));
#3299=DIRECTION('center_axis',(-4.10284931589583E-15,0.382683432365095,
-0.923879532511285));
#3300=DIRECTION('ref_axis',(9.90515446280873E-15,-0.923879532511285,-0.382683432365095));
#3301=DIRECTION('center_axis',(0.,1.,-2.46716227694479E-17));
#3302=DIRECTION('ref_axis',(-0.70710678118654,0.,-0.707106781186555));
#3303=DIRECTION('',(0.,1.,-2.46716227694479E-17));
#3304=DIRECTION('',(0.,-1.,2.46716227694479E-17));
#3305=DIRECTION('center_axis',(0.,0.707106781186548,-0.707106781186548));
#3306=DIRECTION('ref_axis',(-0.707106781186553,0.499999999999996,0.499999999999996));
#3307=DIRECTION('',(0.,0.707106781186548,-0.707106781186548));
#3308=DIRECTION('',(0.,-0.707106781186548,0.707106781186548));
#3309=DIRECTION('center_axis',(-8.497279155086E-16,0.923879532511287,-0.382683432365089));
#3310=DIRECTION('ref_axis',(-2.05142465794788E-15,0.382683432365089,0.923879532511287));
#3311=DIRECTION('center_axis',(0.,-1.,0.));
#3312=DIRECTION('ref_axis',(-0.70710678118654,0.,0.707106781186555));
#3313=DIRECTION('',(0.,1.,0.));
#3314=DIRECTION('',(0.,-1.,0.));
#3315=DIRECTION('center_axis',(0.,1.,0.));
#3316=DIRECTION('ref_axis',(0.,0.,-1.));
#3317=DIRECTION('',(1.,0.,0.));
#3318=DIRECTION('',(0.,0.,-1.));
#3319=DIRECTION('',(-1.,0.,0.));
#3320=DIRECTION('center_axis',(0.,0.707106781186547,0.707106781186548));
#3321=DIRECTION('ref_axis',(1.,0.,0.));
#3322=DIRECTION('',(-1.,0.,0.));
#3323=DIRECTION('',(0.,0.707106781186548,-0.707106781186547));
#3324=DIRECTION('center_axis',(0.,2.46716227694479E-17,1.));
#3325=DIRECTION('ref_axis',(0.,1.,-2.46716227694479E-17));
#3326=DIRECTION('',(1.,0.,0.));
#3327=DIRECTION('',(0.,1.,-2.46716227694479E-17));
#3328=DIRECTION('center_axis',(0.,-0.707106781186548,0.707106781186548));
#3329=DIRECTION('ref_axis',(1.,0.,0.));
#3330=DIRECTION('',(-1.,0.,0.));
#3331=DIRECTION('',(0.,0.707106781186548,0.707106781186548));
#3332=DIRECTION('center_axis',(1.,0.,0.));
#3333=DIRECTION('ref_axis',(0.,0.,-1.));
#3334=DIRECTION('center_axis',(0.,-0.707106781186548,-0.707106781186548));
#3335=DIRECTION('ref_axis',(-1.,0.,0.));
#3336=DIRECTION('',(-1.,0.,0.));
#3337=DIRECTION('',(0.,-0.707106781186548,0.707106781186548));
#3338=DIRECTION('',(1.,0.,0.));
#3339=DIRECTION('center_axis',(0.,-1.,0.));
#3340=DIRECTION('ref_axis',(0.,0.,1.));
#3341=DIRECTION('',(0.,0.,1.));
#3342=DIRECTION('center_axis',(0.,0.707106781186548,-0.707106781186548));
#3343=DIRECTION('ref_axis',(-1.,0.,0.));
#3344=DIRECTION('',(0.,-0.707106781186548,-0.707106781186548));
#3345=DIRECTION('',(1.,0.,0.));
#3346=DIRECTION('center_axis',(0.,0.,-1.));
#3347=DIRECTION('ref_axis',(0.,-1.,0.));
#3348=DIRECTION('',(0.,-1.,0.));
#3349=DIRECTION('center_axis',(1.,0.,0.));
#3350=DIRECTION('ref_axis',(0.,1.,0.));
#3351=DIRECTION('axis',(0.,0.,1.));
#3352=DIRECTION('refdir',(1.,0.,0.));
#3353=DIRECTION('center_axis',(0.,0.707106781186548,0.707106781186548));
#3354=DIRECTION('ref_axis',(0.707106781186541,-0.500000000000005,0.500000000000005));
#3355=DIRECTION('',(0.,0.707106781186548,0.707106781186548));
#3356=DIRECTION('center_axis',(0.,-0.923879532511287,-0.38268343236509));
#3357=DIRECTION('ref_axis',(0.,0.38268343236509,-0.923879532511287));
#3358=DIRECTION('',(0.,-0.707106781186548,-0.707106781186548));
#3359=DIRECTION('center_axis',(-2.05142465794792E-15,-0.382683432365092,
-0.923879532511286));
#3360=DIRECTION('ref_axis',(4.95257723140443E-15,0.923879532511286,-0.382683432365092));
#3361=DIRECTION('center_axis',(0.,1.,0.));
#3362=DIRECTION('ref_axis',(0.70710678118654,0.,0.707106781186555));
#3363=DIRECTION('',(0.,1.,0.));
#3364=DIRECTION('center_axis',(4.24863957754293E-15,-0.923879532511293,
0.382683432365076));
#3365=DIRECTION('ref_axis',(-1.02571232897397E-14,-0.382683432365076,-0.923879532511292));
#3366=DIRECTION('',(0.,-1.,0.));
#3367=DIRECTION('center_axis',(0.,0.,-1.));
#3368=DIRECTION('ref_axis',(0.707106781186548,0.707106781186548,0.));
#3369=DIRECTION('',(0.,0.,1.));
#3370=DIRECTION('center_axis',(0.,0.382683432365083,-0.92387953251129));
#3371=DIRECTION('ref_axis',(0.,0.92387953251129,0.382683432365083));
#3372=DIRECTION('',(0.,0.,-1.));
#3373=DIRECTION('center_axis',(0.,0.382683432365092,0.923879532511286));
#3374=DIRECTION('ref_axis',(0.,-0.923879532511286,0.382683432365092));
#3375=DIRECTION('center_axis',(0.,0.707106781186547,-0.707106781186548));
#3376=DIRECTION('ref_axis',(0.707106781186543,0.500000000000006,0.5));
#3377=DIRECTION('',(0.,0.707106781186547,-0.707106781186548));
#3378=DIRECTION('',(0.,-0.707106781186547,0.707106781186548));
#3379=DIRECTION('center_axis',(0.,-0.707106781186548,-0.707106781186548));
#3380=DIRECTION('ref_axis',(0.707106781186541,0.500000000000005,-0.500000000000005));
#3381=DIRECTION('',(0.,0.707106781186548,0.707106781186548));
#3382=DIRECTION('',(0.,-0.707106781186548,-0.707106781186548));
#3383=DIRECTION('center_axis',(0.,0.923879532511293,0.382683432365075));
#3384=DIRECTION('ref_axis',(0.,-0.382683432365075,0.923879532511293));
#3385=DIRECTION('center_axis',(0.,-1.,2.61228946970625E-17));
#3386=DIRECTION('ref_axis',(0.70710678118654,0.,-0.707106781186555));
#3387=DIRECTION('',(0.,1.,-2.61228946970625E-17));
#3388=DIRECTION('',(0.,-1.,2.61228946970625E-17));
#3389=DIRECTION('center_axis',(-1.7261125179092E-14,0.923879532511293,-0.382683432365076));
#3390=DIRECTION('ref_axis',(4.16720425091855E-14,0.382683432365076,0.923879532511292));
#3391=DIRECTION('center_axis',(0.,-0.707106781186548,0.707106781186547));
#3392=DIRECTION('ref_axis',(0.707106781186541,-0.500000000000005,-0.500000000000005));
#3393=DIRECTION('',(0.,0.707106781186548,-0.707106781186547));
#3394=DIRECTION('',(0.,-0.707106781186548,0.707106781186547));
#3395=DIRECTION('center_axis',(0.,0.382683432365092,-0.923879532511286));
#3396=DIRECTION('ref_axis',(0.,0.923879532511286,0.382683432365092));
#3397=DIRECTION('center_axis',(0.,0.,1.));
#3398=DIRECTION('ref_axis',(0.707106781186548,-0.707106781186548,0.));
#3399=DIRECTION('',(0.,0.,-1.));
#3400=DIRECTION('',(0.,0.,1.));
#3401=DIRECTION('center_axis',(0.,-0.707106781186548,0.707106781186548));
#3402=DIRECTION('ref_axis',(0.,0.707106781186548,0.707106781186548));
#3403=DIRECTION('',(-1.,0.,0.));
#3404=DIRECTION('',(0.,0.707106781186547,0.707106781186547));
#3405=DIRECTION('',(-1.,0.,0.));
#3406=DIRECTION('center_axis',(0.,0.,1.));
#3407=DIRECTION('ref_axis',(0.,1.,0.));
#3408=DIRECTION('',(-1.,0.,0.));
#3409=DIRECTION('',(0.,-1.,0.));
#3410=DIRECTION('',(-1.,0.,0.));
#3411=DIRECTION('',(0.,1.,0.));
#3412=DIRECTION('center_axis',(0.,0.707106781186548,0.707106781186547));
#3413=DIRECTION('ref_axis',(0.,0.707106781186547,-0.707106781186548));
#3414=DIRECTION('',(-1.,0.,0.));
#3415=DIRECTION('',(0.,-0.707106781186547,0.707106781186548));
#3416=DIRECTION('center_axis',(0.,1.,0.));
#3417=DIRECTION('ref_axis',(0.,0.,-1.));
#3418=DIRECTION('',(-1.,0.,0.));
#3419=DIRECTION('',(0.,0.,1.));
#3420=DIRECTION('center_axis',(-1.,0.,0.));
#3421=DIRECTION('ref_axis',(0.,-1.,0.));
#3422=DIRECTION('center_axis',(0.,-1.,0.));
#3423=DIRECTION('ref_axis',(0.,0.,-1.));
#3424=DIRECTION('',(0.,0.,-1.));
#3425=DIRECTION('',(0.,0.,-1.));
#3426=DIRECTION('',(1.,0.,0.));
#3427=DIRECTION('center_axis',(1.,0.,0.));
#3428=DIRECTION('ref_axis',(0.,0.,-1.));
#3429=DIRECTION('',(0.,0.707106781186548,0.707106781186548));
#3430=DIRECTION('',(0.,1.,-2.61228946970625E-17));
#3431=DIRECTION('center_axis',(0.,0.707106781186548,-0.707106781186548));
#3432=DIRECTION('ref_axis',(0.,-0.707106781186548,-0.707106781186548));
#3433=DIRECTION('',(-1.,0.,0.));
#3434=DIRECTION('center_axis',(0.,-1.,0.));
#3435=DIRECTION('ref_axis',(0.,0.,1.));
#3436=DIRECTION('',(0.,0.,1.));
#3437=DIRECTION('',(-1.,0.,0.));
#3438=DIRECTION('center_axis',(0.,-0.707106781186547,-0.707106781186548));
#3439=DIRECTION('ref_axis',(0.,-0.707106781186548,0.707106781186547));
#3440=DIRECTION('',(0.,-0.707106781186548,0.707106781186547));
#3441=DIRECTION('',(-1.,0.,0.));
#3442=DIRECTION('center_axis',(0.,-2.61228946970625E-17,-1.));
#3443=DIRECTION('ref_axis',(0.,-1.,2.61228946970625E-17));
#3444=DIRECTION('',(0.,-1.,2.61228946970625E-17));
#3445=DIRECTION('center_axis',(-1.,0.,0.));
#3446=DIRECTION('ref_axis',(0.,0.,1.));
#3447=DIRECTION('axis',(0.,0.,1.));
#3448=DIRECTION('refdir',(1.,0.,0.));
#3449=DIRECTION('center_axis',(-1.,0.,0.));
#3450=DIRECTION('ref_axis',(0.,-1.,0.));
#3451=DIRECTION('center_axis',(-1.,0.,0.));
#3452=DIRECTION('ref_axis',(0.,-1.,0.));
#3453=DIRECTION('',(1.,0.,0.));
#3454=DIRECTION('center_axis',(1.,0.,0.));
#3455=DIRECTION('ref_axis',(0.,-1.,0.));
#3456=DIRECTION('center_axis',(-1.,0.,0.));
#3457=DIRECTION('ref_axis',(0.,-1.,0.));
#3458=DIRECTION('center_axis',(1.,0.,0.));
#3459=DIRECTION('ref_axis',(0.,-1.,0.));
#3460=DIRECTION('',(1.,0.,0.));
#3461=DIRECTION('center_axis',(1.,0.,0.));
#3462=DIRECTION('ref_axis',(0.,-1.,0.));
#3463=DIRECTION('center_axis',(-1.,0.,0.));
#3464=DIRECTION('ref_axis',(0.,-1.,0.));
#3465=DIRECTION('center_axis',(-1.,0.,0.));
#3466=DIRECTION('ref_axis',(0.,-1.,0.));
#3467=DIRECTION('center_axis',(-1.,0.,0.));
#3468=DIRECTION('ref_axis',(0.,-1.,0.));
#3469=DIRECTION('',(1.,0.,0.));
#3470=DIRECTION('center_axis',(-1.,0.,0.));
#3471=DIRECTION('ref_axis',(0.,-1.,0.));
#3472=DIRECTION('center_axis',(-1.,0.,0.));
#3473=DIRECTION('ref_axis',(0.,-1.,0.));
#3474=DIRECTION('center_axis',(-1.,0.,0.));
#3475=DIRECTION('ref_axis',(0.,-1.,0.));
#3476=DIRECTION('axis',(0.,0.,1.));
#3477=DIRECTION('refdir',(1.,0.,0.));
#3478=DIRECTION('center_axis',(0.,1.,0.));
#3479=DIRECTION('ref_axis',(-1.,0.,0.));
#3480=DIRECTION('',(1.,0.,0.));
#3481=DIRECTION('',(0.,0.,1.));
#3482=DIRECTION('',(-1.,0.,0.));
#3483=DIRECTION('',(0.,0.,1.));
#3484=DIRECTION('center_axis',(0.,0.,1.));
#3485=DIRECTION('ref_axis',(1.,0.,0.));
#3486=DIRECTION('',(0.,-1.,0.));
#3487=DIRECTION('',(1.,0.,0.));
#3488=DIRECTION('',(0.,1.,0.));
#3489=DIRECTION('center_axis',(0.,0.,1.));
#3490=DIRECTION('ref_axis',(0.,1.,0.));
#3491=DIRECTION('',(0.,1.,0.));
#3492=DIRECTION('',(-1.,0.,0.));
#3493=DIRECTION('',(0.,1.,0.));
#3494=DIRECTION('center_axis',(0.,-1.,0.));
#3495=DIRECTION('ref_axis',(1.,0.,0.));
#3496=DIRECTION('',(0.,0.,1.));
#3497=DIRECTION('',(1.,0.,0.));
#3498=DIRECTION('',(0.,0.,1.));
#3499=DIRECTION('center_axis',(0.,0.,1.));
#3500=DIRECTION('ref_axis',(1.,0.,0.));
#3501=DIRECTION('',(0.,1.,0.));
#3502=DIRECTION('',(-1.,0.,0.));
#3503=DIRECTION('',(0.,-1.,0.));
#3504=DIRECTION('center_axis',(0.,-1.,0.));
#3505=DIRECTION('ref_axis',(0.,0.,1.));
#3506=DIRECTION('',(0.,0.,1.));
#3507=DIRECTION('',(0.,0.,1.));
#3508=DIRECTION('',(-1.,0.,0.));
#3509=DIRECTION('center_axis',(0.,-0.707106781186547,-0.707106781186548));
#3510=DIRECTION('ref_axis',(0.,-0.707106781186548,0.707106781186547));
#3511=DIRECTION('',(0.,-0.707106781186548,0.707106781186547));
#3512=DIRECTION('',(0.,-0.707106781186548,0.707106781186547));
#3513=DIRECTION('',(-1.,0.,0.));
#3514=DIRECTION('center_axis',(0.,0.,-1.));
#3515=DIRECTION('ref_axis',(0.,-1.,0.));
#3516=DIRECTION('',(0.,-1.,0.));
#3517=DIRECTION('',(0.,-1.,0.));
#3518=DIRECTION('',(-1.,0.,0.));
#3519=DIRECTION('center_axis',(0.,1.,0.));
#3520=DIRECTION('ref_axis',(0.,0.,-1.));
#3521=DIRECTION('',(0.,0.,-1.));
#3522=DIRECTION('',(0.,0.,1.));
#3523=DIRECTION('center_axis',(-1.,0.,0.));
#3524=DIRECTION('ref_axis',(0.,0.,1.));
#3525=DIRECTION('center_axis',(-1.,0.,0.));
#3526=DIRECTION('ref_axis',(0.,-1.,0.));
#3527=DIRECTION('axis',(0.,0.,1.));
#3528=DIRECTION('refdir',(1.,0.,0.));
#3529=DIRECTION('center_axis',(0.,0.,-1.));
#3530=DIRECTION('ref_axis',(-1.,0.,0.));
#3531=DIRECTION('center_axis',(0.,0.,-1.));
#3532=DIRECTION('ref_axis',(-1.,0.,0.));
#3533=DIRECTION('',(0.,0.,-1.));
#3534=DIRECTION('center_axis',(0.,0.,-1.));
#3535=DIRECTION('ref_axis',(-1.,0.,0.));
#3536=DIRECTION('',(0.,0.,-1.));
#3537=DIRECTION('center_axis',(0.,0.,1.));
#3538=DIRECTION('ref_axis',(-1.,0.,0.));
#3539=DIRECTION('center_axis',(0.,0.,-1.));
#3540=DIRECTION('ref_axis',(-1.,0.,0.));
#3541=DIRECTION('center_axis',(0.,0.,-1.));
#3542=DIRECTION('ref_axis',(-1.,0.,0.));
#3543=DIRECTION('',(0.,0.,-1.));
#3544=DIRECTION('center_axis',(0.,0.,1.));
#3545=DIRECTION('ref_axis',(-1.,0.,0.));
#3546=DIRECTION('center_axis',(0.,0.,-1.));
#3547=DIRECTION('ref_axis',(-1.,0.,0.));
#3548=DIRECTION('center_axis',(0.,0.,-1.));
#3549=DIRECTION('ref_axis',(-1.,0.,0.));
#3550=DIRECTION('',(0.,0.,-1.));
#3551=DIRECTION('center_axis',(0.,0.,1.));
#3552=DIRECTION('ref_axis',(-1.,0.,0.));
#3553=DIRECTION('center_axis',(0.,0.,-1.));
#3554=DIRECTION('ref_axis',(-1.,0.,0.));
#3555=DIRECTION('center_axis',(0.,0.,-1.));
#3556=DIRECTION('ref_axis',(-1.,0.,0.));
#3557=DIRECTION('',(0.,0.,-1.));
#3558=DIRECTION('center_axis',(0.,0.,-1.));
#3559=DIRECTION('ref_axis',(-1.,0.,0.));
#3560=DIRECTION('',(0.,0.,-1.));
#3561=DIRECTION('center_axis',(0.,0.,1.));
#3562=DIRECTION('ref_axis',(-1.,0.,0.));
#3563=DIRECTION('center_axis',(0.,0.,-1.));
#3564=DIRECTION('ref_axis',(-1.,0.,0.));
#3565=DIRECTION('center_axis',(0.,0.,-1.));
#3566=DIRECTION('ref_axis',(-1.,0.,0.));
#3567=DIRECTION('',(0.,0.,-1.));
#3568=DIRECTION('center_axis',(0.,0.,1.));
#3569=DIRECTION('ref_axis',(-1.,0.,0.));
#3570=DIRECTION('center_axis',(0.,0.,-1.));
#3571=DIRECTION('ref_axis',(-1.,0.,0.));
#3572=DIRECTION('center_axis',(0.,0.,-1.));
#3573=DIRECTION('ref_axis',(-1.,0.,0.));
#3574=DIRECTION('',(0.,0.,-1.));
#3575=DIRECTION('center_axis',(0.,0.,1.));
#3576=DIRECTION('ref_axis',(-1.,0.,0.));
#3577=DIRECTION('center_axis',(-0.816496580927728,0.408248290463864,0.408248290463857));
#3578=DIRECTION('ref_axis',(0.57735026918962,0.577350269189634,0.577350269189623));
#3579=DIRECTION('center_axis',(0.,1.,-1.77635683940025E-14));
#3580=DIRECTION('ref_axis',(1.,0.,0.));
#3581=DIRECTION('center_axis',(0.,0.,1.));
#3582=DIRECTION('ref_axis',(0.,1.,0.));
#3583=DIRECTION('center_axis',(1.,-4.44089209850064E-15,0.));
#3584=DIRECTION('ref_axis',(0.,0.,1.));
#3585=DIRECTION('center_axis',(0.,0.,1.));
#3586=DIRECTION('ref_axis',(0.707106781186544,0.707106781186551,0.));
#3587=DIRECTION('center_axis',(0.,0.,1.));
#3588=DIRECTION('ref_axis',(0.707106781186544,0.707106781186551,0.));
#3589=DIRECTION('',(0.,0.,1.));
#3590=DIRECTION('',(0.,0.,-1.));
#3591=DIRECTION('center_axis',(-0.408248290463861,-0.816496580927726,0.408248290463865));
#3592=DIRECTION('ref_axis',(-0.577350269189626,0.577350269189626,0.577350269189626));
#3593=DIRECTION('center_axis',(-1.,0.,0.));
#3594=DIRECTION('ref_axis',(0.,1.,0.));
#3595=DIRECTION('center_axis',(0.,0.,1.));
#3596=DIRECTION('ref_axis',(-1.,0.,0.));
#3597=DIRECTION('center_axis',(0.,1.,0.));
#3598=DIRECTION('ref_axis',(0.,0.,1.));
#3599=DIRECTION('center_axis',(0.,0.,1.));
#3600=DIRECTION('ref_axis',(-0.707106781186548,0.707106781186548,0.));
#3601=DIRECTION('center_axis',(0.,0.,1.));
#3602=DIRECTION('ref_axis',(-0.707106781186548,0.707106781186548,0.));
#3603=DIRECTION('',(0.,0.,1.));
#3604=DIRECTION('',(0.,0.,-1.));
#3605=DIRECTION('center_axis',(-0.816496580927733,-0.408248290463861,0.408248290463851));
#3606=DIRECTION('ref_axis',(0.577350269189619,-0.57735026918964,0.577350269189619));
#3607=DIRECTION('center_axis',(1.,0.,0.));
#3608=DIRECTION('ref_axis',(0.,-1.,0.));
#3609=DIRECTION('center_axis',(0.,0.,1.));
#3610=DIRECTION('ref_axis',(1.,0.,0.));
#3611=DIRECTION('center_axis',(1.77635683940025E-14,-1.,0.));
#3612=DIRECTION('ref_axis',(0.,0.,1.));
#3613=DIRECTION('center_axis',(0.,0.,1.));
#3614=DIRECTION('ref_axis',(0.707106781186541,-0.707106781186554,0.));
#3615=DIRECTION('center_axis',(0.,0.,1.));
#3616=DIRECTION('ref_axis',(0.707106781186541,-0.707106781186554,0.));
#3617=DIRECTION('',(0.,0.,1.));
#3618=DIRECTION('',(0.,0.,-1.));
#3619=DIRECTION('center_axis',(0.,1.,0.));
#3620=DIRECTION('ref_axis',(0.707106781186549,0.,0.707106781186546));
#3621=DIRECTION('',(0.,-1.,0.));
#3622=DIRECTION('',(0.,1.,0.));
#3623=DIRECTION('center_axis',(0.408248290463862,-0.816496580927725,-0.408248290463866));
#3624=DIRECTION('ref_axis',(-0.577350269189626,-0.577350269189626,0.577350269189626));
#3625=DIRECTION('center_axis',(0.,-1.,0.));
#3626=DIRECTION('ref_axis',(-1.,0.,0.));
#3627=DIRECTION('center_axis',(0.,0.,1.));
#3628=DIRECTION('ref_axis',(0.,-1.,0.));
#3629=DIRECTION('center_axis',(-1.,0.,0.));
#3630=DIRECTION('ref_axis',(0.,0.,1.));
#3631=DIRECTION('center_axis',(0.,0.,1.));
#3632=DIRECTION('ref_axis',(-0.707106781186554,-0.707106781186541,0.));
#3633=DIRECTION('center_axis',(0.,0.,1.));
#3634=DIRECTION('ref_axis',(-0.707106781186554,-0.707106781186541,0.));
#3635=DIRECTION('',(0.,0.,1.));
#3636=DIRECTION('',(0.,0.,-1.));
#3637=DIRECTION('center_axis',(1.,0.,0.));
#3638=DIRECTION('ref_axis',(0.,-0.70710678118654,0.707106781186555));
#3639=DIRECTION('',(-1.,0.,0.));
#3640=DIRECTION('',(1.,0.,0.));
#3641=DIRECTION('center_axis',(0.,-1.,0.));
#3642=DIRECTION('ref_axis',(-0.707106781186546,0.,0.707106781186549));
#3643=DIRECTION('',(0.,1.,0.));
#3644=DIRECTION('',(0.,-1.,0.));
#3645=DIRECTION('center_axis',(-1.,0.,0.));
#3646=DIRECTION('ref_axis',(0.,0.707106781186546,0.707106781186549));
#3647=DIRECTION('',(1.,0.,0.));
#3648=DIRECTION('',(-1.,0.,0.));
#3649=DIRECTION('center_axis',(1.,0.,0.));
#3650=DIRECTION('ref_axis',(0.,1.,0.));
#3651=DIRECTION('',(0.,1.,0.));
#3652=DIRECTION('',(0.,0.,1.));
#3653=DIRECTION('',(0.,1.,0.));
#3654=DIRECTION('',(0.,0.,-1.));
#3655=DIRECTION('',(0.,1.,0.));
#3656=DIRECTION('',(0.,0.,-1.));
#3657=DIRECTION('',(0.,-1.,0.));
#3658=DIRECTION('',(0.,0.,1.));
#3659=DIRECTION('',(0.,1.,0.));
#3660=DIRECTION('',(0.,0.,1.));
#3661=DIRECTION('',(0.,1.,0.));
#3662=DIRECTION('',(0.,0.,-1.));
#3663=DIRECTION('',(0.,1.,0.));
#3664=DIRECTION('center_axis',(-1.,0.,0.));
#3665=DIRECTION('ref_axis',(0.,-1.,0.));
#3666=DIRECTION('center_axis',(0.,-1.,0.));
#3667=DIRECTION('ref_axis',(1.,0.,0.));
#3668=DIRECTION('',(1.,0.,0.));
#3669=DIRECTION('center_axis',(0.,0.,1.));
#3670=DIRECTION('ref_axis',(1.,0.,0.));
#3671=DIRECTION('',(0.,-1.,0.));
#3672=DIRECTION('',(1.,0.,0.));
#3673=DIRECTION('center_axis',(0.,0.,1.));
#3674=DIRECTION('ref_axis',(1.,0.,0.));
#3675=DIRECTION('center_axis',(-1.,0.,0.));
#3676=DIRECTION('ref_axis',(0.,-1.,0.));
#3677=DIRECTION('',(-1.,0.,0.));
#3678=DIRECTION('center_axis',(1.,0.,0.));
#3679=DIRECTION('ref_axis',(0.,-1.,0.));
#3680=DIRECTION('center_axis',(0.,-1.,0.));
#3681=DIRECTION('ref_axis',(1.,0.,0.));
#3682=DIRECTION('',(0.,0.,-1.));
#3683=DIRECTION('',(1.,0.,0.));
#3684=DIRECTION('',(1.,0.,0.));
#3685=DIRECTION('center_axis',(0.,1.,0.));
#3686=DIRECTION('ref_axis',(-1.,0.,0.));
#3687=DIRECTION('',(0.,0.,1.));
#3688=DIRECTION('',(-1.,0.,0.));
#3689=DIRECTION('',(-1.,0.,0.));
#3690=DIRECTION('center_axis',(0.,0.,1.));
#3691=DIRECTION('ref_axis',(1.,0.,0.));
#3692=DIRECTION('',(0.,-1.,0.));
#3693=DIRECTION('center_axis',(0.,-1.,0.));
#3694=DIRECTION('ref_axis',(1.,0.,0.));
#3695=DIRECTION('',(0.,0.,-1.));
#3696=DIRECTION('',(1.,0.,0.));
#3697=DIRECTION('center_axis',(0.,1.,0.));
#3698=DIRECTION('ref_axis',(-1.,0.,0.));
#3699=DIRECTION('',(0.,0.,1.));
#3700=DIRECTION('',(-1.,0.,0.));
#3701=DIRECTION('',(-1.,0.,0.));
#3702=DIRECTION('center_axis',(0.,0.,1.));
#3703=DIRECTION('ref_axis',(1.,0.,0.));
#3704=DIRECTION('',(0.,-1.,0.));
#3705=DIRECTION('center_axis',(0.,0.,1.));
#3706=DIRECTION('ref_axis',(1.,0.,0.));
#3707=DIRECTION('',(0.,-1.,0.));
#3708=DIRECTION('',(-1.,0.,0.));
#3709=DIRECTION('center_axis',(0.,0.,1.));
#3710=DIRECTION('ref_axis',(1.,0.,0.));
#3711=DIRECTION('',(0.,-1.,0.));
#3712=DIRECTION('',(-1.,0.,0.));
#3713=DIRECTION('center_axis',(0.,0.,1.));
#3714=DIRECTION('ref_axis',(1.,0.,0.));
#3715=DIRECTION('',(1.,0.,0.));
#3716=DIRECTION('',(0.,-1.,0.));
#3717=DIRECTION('center_axis',(0.,-1.,0.));
#3718=DIRECTION('ref_axis',(1.,0.,0.));
#3719=DIRECTION('',(0.,0.,-1.));
#3720=DIRECTION('',(1.,0.,0.));
#3721=DIRECTION('center_axis',(0.,1.,0.));
#3722=DIRECTION('ref_axis',(-1.,0.,0.));
#3723=DIRECTION('',(0.,0.,1.));
#3724=DIRECTION('',(-1.,0.,0.));
#3725=DIRECTION('center_axis',(-1.,0.,0.));
#3726=DIRECTION('ref_axis',(0.,-1.,0.));
#3727=DIRECTION('',(0.,1.,0.));
#3728=DIRECTION('center_axis',(0.,0.,1.));
#3729=DIRECTION('ref_axis',(-1.,0.,0.));
#3730=DIRECTION('center_axis',(0.,1.,0.));
#3731=DIRECTION('ref_axis',(-1.,0.,0.));
#3732=DIRECTION('axis',(0.,0.,1.));
#3733=DIRECTION('refdir',(1.,0.,0.));
#3734=DIRECTION('center_axis',(1.,0.,0.));
#3735=DIRECTION('ref_axis',(0.,1.,0.));
#3736=DIRECTION('center_axis',(1.,0.,0.));
#3737=DIRECTION('ref_axis',(0.,1.,0.));
#3738=DIRECTION('',(-1.,0.,0.));
#3739=DIRECTION('center_axis',(-1.,0.,0.));
#3740=DIRECTION('ref_axis',(0.,1.,0.));
#3741=DIRECTION('center_axis',(1.,0.,0.));
#3742=DIRECTION('ref_axis',(0.,1.,0.));
#3743=DIRECTION('center_axis',(0.,0.707106781186548,-0.707106781186548));
#3744=DIRECTION('ref_axis',(-1.,0.,0.));
#3745=DIRECTION('',(0.,-0.707106781186548,-0.707106781186548));
#3746=DIRECTION('',(-1.,0.,0.));
#3747=DIRECTION('',(0.,0.707106781186548,0.707106781186548));
#3748=DIRECTION('',(1.,0.,0.));
#3749=DIRECTION('center_axis',(1.,0.,0.));
#3750=DIRECTION('ref_axis',(0.,1.,0.));
#3751=DIRECTION('',(0.,-1.,3.70074341541719E-17));
#3752=DIRECTION('',(0.,0.707106781186548,-0.707106781186548));
#3753=DIRECTION('',(0.,0.,1.));
#3754=DIRECTION('',(0.,-0.707106781186548,-0.707106781186548));
#3755=DIRECTION('',(0.,1.,0.));
#3756=DIRECTION('',(0.,-0.707106781186548,0.707106781186548));
#3757=DIRECTION('',(0.,0.,-1.));
#3758=DIRECTION('center_axis',(0.,-3.70074341541719E-17,-1.));
#3759=DIRECTION('ref_axis',(0.,1.,-3.70074341541719E-17));
#3760=DIRECTION('',(0.,1.,-3.70074341541719E-17));
#3761=DIRECTION('',(1.,0.,0.));
#3762=DIRECTION('center_axis',(0.,-0.707106781186548,-0.707106781186548));
#3763=DIRECTION('ref_axis',(-1.,0.,0.));
#3764=DIRECTION('',(0.,-0.707106781186548,0.707106781186548));
#3765=DIRECTION('',(-1.,0.,0.));
#3766=DIRECTION('center_axis',(0.,0.707106781186548,0.707106781186548));
#3767=DIRECTION('ref_axis',(1.,0.,0.));
#3768=DIRECTION('',(0.,0.707106781186548,-0.707106781186548));
#3769=DIRECTION('',(-1.,0.,0.));
#3770=DIRECTION('',(1.,0.,0.));
#3771=DIRECTION('center_axis',(0.,0.,1.));
#3772=DIRECTION('ref_axis',(0.,-1.,0.));
#3773=DIRECTION('',(-1.,0.,0.));
#3774=DIRECTION('',(0.,-1.,0.));
#3775=DIRECTION('center_axis',(0.,-0.707106781186548,0.707106781186548));
#3776=DIRECTION('ref_axis',(1.,0.,0.));
#3777=DIRECTION('',(0.,0.707106781186548,0.707106781186548));
#3778=DIRECTION('',(1.,0.,0.));
#3779=DIRECTION('center_axis',(0.,-1.,0.));
#3780=DIRECTION('ref_axis',(0.,0.,-1.));
#3781=DIRECTION('',(0.,0.,-1.));
#3782=DIRECTION('center_axis',(0.,1.,0.));
#3783=DIRECTION('ref_axis',(0.,0.,1.));
#3784=DIRECTION('',(0.,0.,1.));
#3785=DIRECTION('center_axis',(1.,0.,0.));
#3786=DIRECTION('ref_axis',(0.,0.,-1.));
#3787=DIRECTION('axis',(0.,0.,1.));
#3788=DIRECTION('refdir',(1.,0.,0.));
#3789=DIRECTION('center_axis',(-1.,0.,0.));
#3790=DIRECTION('ref_axis',(0.,-1.,0.));
#3791=DIRECTION('center_axis',(-1.,0.,0.));
#3792=DIRECTION('ref_axis',(0.,-1.,0.));
#3793=DIRECTION('',(-1.,0.,0.));
#3794=DIRECTION('center_axis',(1.,0.,0.));
#3795=DIRECTION('ref_axis',(0.,-1.,0.));
#3796=DIRECTION('center_axis',(-1.,0.,0.));
#3797=DIRECTION('ref_axis',(0.,-1.,0.));
#3798=DIRECTION('center_axis',(1.,0.,0.));
#3799=DIRECTION('ref_axis',(0.,-1.,0.));
#3800=DIRECTION('',(-1.,0.,0.));
#3801=DIRECTION('center_axis',(1.,0.,0.));
#3802=DIRECTION('ref_axis',(0.,-1.,0.));
#3803=DIRECTION('center_axis',(-1.,0.,0.));
#3804=DIRECTION('ref_axis',(0.,-1.,0.));
#3805=DIRECTION('center_axis',(-1.,0.,0.));
#3806=DIRECTION('ref_axis',(0.,-1.,0.));
#3807=DIRECTION('center_axis',(-1.,0.,0.));
#3808=DIRECTION('ref_axis',(0.,-1.,0.));
#3809=DIRECTION('',(-1.,0.,0.));
#3810=DIRECTION('center_axis',(-1.,0.,0.));
#3811=DIRECTION('ref_axis',(0.,-1.,0.));
#3812=DIRECTION('center_axis',(-1.,0.,0.));
#3813=DIRECTION('ref_axis',(0.,-1.,0.));
#3814=DIRECTION('center_axis',(-1.,0.,0.));
#3815=DIRECTION('ref_axis',(0.,-1.,0.));
#3816=DIRECTION('axis',(0.,0.,1.));
#3817=DIRECTION('refdir',(1.,0.,0.));
#3818=DIRECTION('center_axis',(0.,0.707106781186548,-0.707106781186548));
#3819=DIRECTION('ref_axis',(-1.,0.,0.));
#3820=DIRECTION('',(0.,-0.707106781186548,-0.707106781186548));
#3821=DIRECTION('',(-1.,0.,0.));
#3822=DIRECTION('',(0.,0.707106781186548,0.707106781186548));
#3823=DIRECTION('',(1.,0.,0.));
#3824=DIRECTION('center_axis',(0.,-2.46716227694479E-17,-1.));
#3825=DIRECTION('ref_axis',(0.,1.,-2.46716227694479E-17));
#3826=DIRECTION('',(0.,1.,-2.46716227694479E-17));
#3827=DIRECTION('',(1.,0.,0.));
#3828=DIRECTION('',(0.,1.,-2.46716227694479E-17));
#3829=DIRECTION('center_axis',(1.,0.,0.));
#3830=DIRECTION('ref_axis',(0.,0.,-1.));
#3831=DIRECTION('',(0.,0.,1.));
#3832=DIRECTION('',(0.,0.707106781186548,-0.707106781186548));
#3833=DIRECTION('',(0.,-1.,0.));
#3834=DIRECTION('',(0.,0.707106781186548,0.707106781186548));
#3835=DIRECTION('',(0.,0.,-1.));
#3836=DIRECTION('',(0.,-0.707106781186548,0.707106781186547));
#3837=DIRECTION('center_axis',(0.,-0.707106781186547,-0.707106781186548));
#3838=DIRECTION('ref_axis',(-1.,0.,0.));
#3839=DIRECTION('',(-1.,0.,0.));
#3840=DIRECTION('',(0.,0.707106781186548,-0.707106781186547));
#3841=DIRECTION('center_axis',(0.,-1.,0.));
#3842=DIRECTION('ref_axis',(0.,0.,-1.));
#3843=DIRECTION('',(1.,0.,0.));
#3844=DIRECTION('',(0.,0.,-1.));
#3845=DIRECTION('center_axis',(0.,0.707106781186548,0.707106781186548));
#3846=DIRECTION('ref_axis',(1.,0.,0.));
#3847=DIRECTION('',(-1.,0.,0.));
#3848=DIRECTION('',(0.,-0.707106781186548,0.707106781186548));
#3849=DIRECTION('',(1.,0.,0.));
#3850=DIRECTION('center_axis',(0.,1.,0.));
#3851=DIRECTION('ref_axis',(0.,0.,1.));
#3852=DIRECTION('',(0.,0.,1.));
#3853=DIRECTION('center_axis',(0.,-0.707106781186548,0.707106781186548));
#3854=DIRECTION('ref_axis',(1.,0.,0.));
#3855=DIRECTION('',(-1.,0.,0.));
#3856=DIRECTION('',(0.,-0.707106781186548,-0.707106781186548));
#3857=DIRECTION('center_axis',(0.,0.,1.));
#3858=DIRECTION('ref_axis',(0.,-1.,0.));
#3859=DIRECTION('',(0.,-1.,0.));
#3860=DIRECTION('center_axis',(1.,0.,0.));
#3861=DIRECTION('ref_axis',(0.,1.,0.));
#3862=DIRECTION('',(0.,0.,1.));
#3863=DIRECTION('',(1.,0.,0.));
#3864=DIRECTION('',(0.,0.,1.));
#3865=DIRECTION('',(1.,0.,0.));
#3866=DIRECTION('',(0.,0.,1.));
#3867=DIRECTION('',(1.,0.,0.));
#3868=DIRECTION('',(0.,0.,1.));
#3869=DIRECTION('',(1.,0.,0.));
#3870=DIRECTION('',(0.,0.,1.));
#3871=DIRECTION('',(1.,0.,0.));
#3872=DIRECTION('',(0.,0.,1.));
#3873=DIRECTION('',(1.,0.,0.));
#3874=DIRECTION('',(0.,0.,1.));
#3875=DIRECTION('',(1.,0.,0.));
#3876=DIRECTION('',(0.,0.,1.));
#3877=DIRECTION('',(1.,0.,0.));
#3878=DIRECTION('',(0.,0.,1.));
#3879=DIRECTION('',(1.,0.,0.));
#3880=DIRECTION('',(0.,0.,1.));
#3881=DIRECTION('',(1.,0.,0.));
#3882=DIRECTION('',(4.15608666884192E-17,1.21400292727948E-17,1.));
#3883=DIRECTION('',(1.,-4.81482486096809E-35,-1.38777878078145E-17));
#3884=CARTESIAN_POINT('',(0.,0.,0.));
#3885=CARTESIAN_POINT('',(0.,0.,0.));
#3886=CARTESIAN_POINT('Origin',(-22.,-75.0000000000105,14.0000000000021));
#3887=CARTESIAN_POINT('',(-18.,-75.0000000000105,14.0000000000021));
#3888=CARTESIAN_POINT('Origin',(-22.,-75.0000000000105,14.0000000000021));
#3889=CARTESIAN_POINT('',(-18.,-75.0000000000105,8.00000000000211));
#3890=CARTESIAN_POINT('',(-18.,-75.0000000000105,14.0000000000021));
#3891=CARTESIAN_POINT('Origin',(-22.,-75.0000000000105,8.00000000000211));
#3892=CARTESIAN_POINT('Origin',(-22.,-75.0000000000105,8.00000000000211));
#3893=CARTESIAN_POINT('Origin',(56.,-75.0000000000105,14.0000000000021));
#3894=CARTESIAN_POINT('',(60.,-75.0000000000105,14.0000000000021));
#3895=CARTESIAN_POINT('Origin',(56.,-75.0000000000105,14.0000000000021));
#3896=CARTESIAN_POINT('',(60.,-75.0000000000105,8.00000000000211));
#3897=CARTESIAN_POINT('',(60.,-75.0000000000105,14.0000000000021));
#3898=CARTESIAN_POINT('Origin',(56.,-75.0000000000105,8.00000000000211));
#3899=CARTESIAN_POINT('Origin',(56.,-75.0000000000105,8.00000000000211));
#3900=CARTESIAN_POINT('Origin',(-48.,-75.0000000000105,14.0000000000021));
#3901=CARTESIAN_POINT('',(-44.,-75.0000000000105,14.0000000000021));
#3902=CARTESIAN_POINT('Origin',(-48.,-75.0000000000105,14.0000000000021));
#3903=CARTESIAN_POINT('',(-44.,-75.0000000000105,8.00000000000211));
#3904=CARTESIAN_POINT('',(-44.,-75.0000000000105,14.0000000000021));
#3905=CARTESIAN_POINT('Origin',(-48.,-75.0000000000105,8.00000000000211));
#3906=CARTESIAN_POINT('Origin',(-48.,-75.0000000000105,8.00000000000211));
#3907=CARTESIAN_POINT('Origin',(4.,-75.0000000000105,14.0000000000021));
#3908=CARTESIAN_POINT('',(8.,-75.0000000000105,14.0000000000021));
#3909=CARTESIAN_POINT('Origin',(4.,-75.0000000000105,14.0000000000021));
#3910=CARTESIAN_POINT('',(8.,-75.0000000000105,8.00000000000211));
#3911=CARTESIAN_POINT('',(8.,-75.0000000000105,14.0000000000021));
#3912=CARTESIAN_POINT('Origin',(4.,-75.0000000000105,8.00000000000211));
#3913=CARTESIAN_POINT('Origin',(4.,-75.0000000000105,8.00000000000211));
#3914=CARTESIAN_POINT('Origin',(30.,-75.0000000000105,14.0000000000021));
#3915=CARTESIAN_POINT('',(34.,-75.0000000000105,14.0000000000021));
#3916=CARTESIAN_POINT('Origin',(30.,-75.0000000000105,14.0000000000021));
#3917=CARTESIAN_POINT('',(34.,-75.0000000000105,8.00000000000211));
#3918=CARTESIAN_POINT('',(34.,-75.0000000000105,14.0000000000021));
#3919=CARTESIAN_POINT('Origin',(30.,-75.0000000000105,8.00000000000211));
#3920=CARTESIAN_POINT('Origin',(30.,-75.0000000000105,8.00000000000211));
#3921=CARTESIAN_POINT('Origin',(-74.,-75.0000000000105,14.0000000000021));
#3922=CARTESIAN_POINT('',(-70.,-75.0000000000105,14.0000000000021));
#3923=CARTESIAN_POINT('Origin',(-74.,-75.0000000000105,14.0000000000021));
#3924=CARTESIAN_POINT('',(-70.,-75.0000000000105,8.00000000000211));
#3925=CARTESIAN_POINT('',(-70.,-75.0000000000105,14.0000000000021));
#3926=CARTESIAN_POINT('Origin',(-74.,-75.0000000000105,8.00000000000211));
#3927=CARTESIAN_POINT('Origin',(-74.,-75.0000000000105,8.00000000000211));
#3928=CARTESIAN_POINT('Origin',(70.,-81.0000000000105,4.00000000000212));
#3929=CARTESIAN_POINT('',(70.,-81.0000000000105,4.00000000000212));
#3930=CARTESIAN_POINT('',(70.,-69.0000000000105,4.00000000000212));
#3931=CARTESIAN_POINT('',(70.,-81.0000000000105,4.00000000000212));
#3932=CARTESIAN_POINT('',(70.,-69.0000000000105,14.0000000000021));
#3933=CARTESIAN_POINT('',(70.,-69.0000000000105,4.00000000000212));
#3934=CARTESIAN_POINT('',(70.,-81.0000000000105,14.0000000000021));
#3935=CARTESIAN_POINT('',(70.,-81.0000000000105,14.0000000000021));
#3936=CARTESIAN_POINT('',(70.,-81.0000000000105,4.00000000000212));
#3937=CARTESIAN_POINT('Origin',(-90.,-81.0000000000105,4.00000000000212));
#3938=CARTESIAN_POINT('',(-90.,-81.0000000000105,4.00000000000212));
#3939=CARTESIAN_POINT('',(-90.,-81.0000000000105,4.00000000000212));
#3940=CARTESIAN_POINT('',(-90.,-81.0000000000105,14.0000000000021));
#3941=CARTESIAN_POINT('',(-90.,-81.0000000000105,14.0000000000021));
#3942=CARTESIAN_POINT('',(-90.,-81.0000000000105,4.00000000000212));
#3943=CARTESIAN_POINT('Origin',(-90.,-69.0000000000105,4.00000000000212));
#3944=CARTESIAN_POINT('',(-90.,-69.0000000000105,4.00000000000212));
#3945=CARTESIAN_POINT('',(-90.,-69.0000000000105,4.00000000000212));
#3946=CARTESIAN_POINT('',(-90.,-69.0000000000105,14.0000000000021));
#3947=CARTESIAN_POINT('',(-90.,-69.0000000000105,14.0000000000021));
#3948=CARTESIAN_POINT('',(-90.,-69.0000000000105,4.00000000000212));
#3949=CARTESIAN_POINT('Origin',(70.,-69.0000000000105,4.00000000000212));
#3950=CARTESIAN_POINT('',(70.,-69.0000000000105,4.00000000000212));
#3951=CARTESIAN_POINT('',(70.,-69.0000000000105,14.0000000000021));
#3952=CARTESIAN_POINT('Origin',(-10.,-75.0000000000105,14.0000000000021));
#3953=CARTESIAN_POINT('Origin',(-10.,-75.0000000000105,4.00000000000212));
#3954=CARTESIAN_POINT('',(0.,0.,0.));
#3955=CARTESIAN_POINT('Origin',(56.,14.9999999999895,14.0000000000021));
#3956=CARTESIAN_POINT('',(60.,14.9999999999895,14.0000000000021));
#3957=CARTESIAN_POINT('Origin',(56.,14.9999999999895,14.0000000000021));
#3958=CARTESIAN_POINT('',(60.,14.9999999999895,8.00000000000211));
#3959=CARTESIAN_POINT('',(60.,14.9999999999895,14.0000000000021));
#3960=CARTESIAN_POINT('Origin',(56.,14.9999999999895,8.00000000000211));
#3961=CARTESIAN_POINT('Origin',(56.,14.9999999999895,8.00000000000211));
#3962=CARTESIAN_POINT('Origin',(-48.,14.9999999999895,14.0000000000021));
#3963=CARTESIAN_POINT('',(-44.,14.9999999999895,14.0000000000021));
#3964=CARTESIAN_POINT('Origin',(-48.,14.9999999999895,14.0000000000021));
#3965=CARTESIAN_POINT('',(-44.,14.9999999999895,8.00000000000211));
#3966=CARTESIAN_POINT('',(-44.,14.9999999999895,14.0000000000021));
#3967=CARTESIAN_POINT('Origin',(-48.,14.9999999999895,8.00000000000211));
#3968=CARTESIAN_POINT('Origin',(-48.,14.9999999999895,8.00000000000211));
#3969=CARTESIAN_POINT('Origin',(-22.,14.9999999999895,14.0000000000021));
#3970=CARTESIAN_POINT('',(-18.,14.9999999999895,14.0000000000021));
#3971=CARTESIAN_POINT('Origin',(-22.,14.9999999999895,14.0000000000021));
#3972=CARTESIAN_POINT('',(-18.,14.9999999999895,8.00000000000211));
#3973=CARTESIAN_POINT('',(-18.,14.9999999999895,14.0000000000021));
#3974=CARTESIAN_POINT('Origin',(-22.,14.9999999999895,8.00000000000211));
#3975=CARTESIAN_POINT('Origin',(-22.,14.9999999999895,8.00000000000211));
#3976=CARTESIAN_POINT('Origin',(30.,14.9999999999895,14.0000000000021));
#3977=CARTESIAN_POINT('',(34.,14.9999999999895,14.0000000000021));
#3978=CARTESIAN_POINT('Origin',(30.,14.9999999999895,14.0000000000021));
#3979=CARTESIAN_POINT('',(34.,14.9999999999895,8.00000000000211));
#3980=CARTESIAN_POINT('',(34.,14.9999999999895,14.0000000000021));
#3981=CARTESIAN_POINT('Origin',(30.,14.9999999999895,8.00000000000211));
#3982=CARTESIAN_POINT('Origin',(30.,14.9999999999895,8.00000000000211));
#3983=CARTESIAN_POINT('Origin',(-74.,14.9999999999895,14.0000000000021));
#3984=CARTESIAN_POINT('',(-70.,14.9999999999895,14.0000000000021));
#3985=CARTESIAN_POINT('Origin',(-74.,14.9999999999895,14.0000000000021));
#3986=CARTESIAN_POINT('',(-70.,14.9999999999895,8.00000000000211));
#3987=CARTESIAN_POINT('',(-70.,14.9999999999895,14.0000000000021));
#3988=CARTESIAN_POINT('Origin',(-74.,14.9999999999895,8.00000000000211));
#3989=CARTESIAN_POINT('Origin',(-74.,14.9999999999895,8.00000000000211));
#3990=CARTESIAN_POINT('Origin',(4.,14.9999999999895,14.0000000000021));
#3991=CARTESIAN_POINT('',(8.,14.9999999999895,14.0000000000021));
#3992=CARTESIAN_POINT('Origin',(4.,14.9999999999895,14.0000000000021));
#3993=CARTESIAN_POINT('',(8.,14.9999999999895,8.00000000000211));
#3994=CARTESIAN_POINT('',(8.,14.9999999999895,14.0000000000021));
#3995=CARTESIAN_POINT('Origin',(4.,14.9999999999895,8.00000000000211));
#3996=CARTESIAN_POINT('Origin',(4.,14.9999999999895,8.00000000000211));
#3997=CARTESIAN_POINT('Origin',(70.,8.99999999998948,4.00000000000212));
#3998=CARTESIAN_POINT('',(70.,20.9999999999895,4.00000000000212));
#3999=CARTESIAN_POINT('',(70.,8.99999999998948,4.00000000000212));
#4000=CARTESIAN_POINT('',(70.,20.9999999999895,4.00000000000212));
#4001=CARTESIAN_POINT('',(70.,20.9999999999895,14.0000000000021));
#4002=CARTESIAN_POINT('',(70.,20.9999999999895,4.00000000000212));
#4003=CARTESIAN_POINT('',(70.,8.99999999998948,14.0000000000021));
#4004=CARTESIAN_POINT('',(70.,20.9999999999895,14.0000000000021));
#4005=CARTESIAN_POINT('',(70.,8.99999999998948,4.00000000000212));
#4006=CARTESIAN_POINT('Origin',(-90.,8.99999999998948,4.00000000000212));
#4007=CARTESIAN_POINT('',(-90.,8.99999999998948,4.00000000000212));
#4008=CARTESIAN_POINT('',(70.,8.99999999998948,4.00000000000212));
#4009=CARTESIAN_POINT('',(-90.,8.99999999998948,14.0000000000021));
#4010=CARTESIAN_POINT('',(70.,8.99999999998948,14.0000000000021));
#4011=CARTESIAN_POINT('',(-90.,8.99999999998948,4.00000000000212));
#4012=CARTESIAN_POINT('Origin',(-90.,20.9999999999895,4.00000000000212));
#4013=CARTESIAN_POINT('',(-90.,20.9999999999895,4.00000000000212));
#4014=CARTESIAN_POINT('',(-90.,8.99999999998948,4.00000000000212));
#4015=CARTESIAN_POINT('',(-90.,20.9999999999895,14.0000000000021));
#4016=CARTESIAN_POINT('',(-90.,8.99999999998948,14.0000000000021));
#4017=CARTESIAN_POINT('',(-90.,20.9999999999895,4.00000000000212));
#4018=CARTESIAN_POINT('Origin',(70.,20.9999999999895,4.00000000000212));
#4019=CARTESIAN_POINT('',(-90.,20.9999999999895,4.00000000000212));
#4020=CARTESIAN_POINT('',(-90.,20.9999999999895,14.0000000000021));
#4021=CARTESIAN_POINT('Origin',(-10.,14.9999999999895,14.0000000000021));
#4022=CARTESIAN_POINT('Origin',(-10.,14.9999999999895,4.00000000000212));
#4023=CARTESIAN_POINT('',(0.,0.,0.));
#4024=CARTESIAN_POINT('Origin',(70.,-30.0000000000105,7.00000000000211));
#4025=CARTESIAN_POINT('',(-90.,-24.0000000000105,7.00000000000211));
#4026=CARTESIAN_POINT('Origin',(-90.,-30.0000000000105,7.00000000000211));
#4027=CARTESIAN_POINT('',(70.,-24.0000000000105,7.00000000000211));
#4028=CARTESIAN_POINT('',(70.,-24.0000000000105,7.00000000000211));
#4029=CARTESIAN_POINT('Origin',(70.,-30.0000000000105,7.00000000000211));
#4030=CARTESIAN_POINT('Origin',(-90.,-30.0000000000105,7.00000000000211));
#4031=CARTESIAN_POINT('Origin',(70.,-30.0000000000105,7.00000000000211));
#4032=CARTESIAN_POINT('',(0.,0.,0.));
#4033=CARTESIAN_POINT('Origin',(91.,-69.292893218824,34.2928932188156));
#4034=CARTESIAN_POINT('',(90.,-84.5857864376374,19.0000000000021));
#4035=CARTESIAN_POINT('',(90.,-89.0000000000105,14.585786437629));
#4036=CARTESIAN_POINT('',(90.,-69.292893218824,34.2928932188156));
#4037=CARTESIAN_POINT('',(91.,-90.0000000000105,15.0000000000021));
#4038=CARTESIAN_POINT('Origin',(91.,-89.0000000000105,14.585786437629));
#4039=CARTESIAN_POINT('',(91.,-85.0000000000105,20.0000000000021));
#4040=CARTESIAN_POINT('',(91.,-70.0000000000105,35.0000000000021));
#4041=CARTESIAN_POINT('Origin',(91.,-84.5857864376374,19.0000000000021));
#4042=CARTESIAN_POINT('Origin',(91.,-89.0000000000105,10.0000000000021));
#4043=CARTESIAN_POINT('',(90.,-89.0000000000105,-14.5857864376248));
#4044=CARTESIAN_POINT('',(90.,-89.0000000000105,10.0000000000021));
#4045=CARTESIAN_POINT('',(91.,-90.0000000000105,-14.9999999999979));
#4046=CARTESIAN_POINT('Origin',(91.,-89.0000000000105,-14.5857864376248));
#4047=CARTESIAN_POINT('',(91.,-90.0000000000105,10.0000000000021));
#4048=CARTESIAN_POINT('Origin',(91.,-69.292893218824,-34.2928932188113));
#4049=CARTESIAN_POINT('',(90.,-84.5857864376374,-18.9999999999979));
#4050=CARTESIAN_POINT('',(90.,-69.292893218824,-34.2928932188113));
#4051=CARTESIAN_POINT('',(91.,-85.0000000000105,-19.9999999999979));
#4052=CARTESIAN_POINT('Origin',(91.,-84.5857864376374,-18.9999999999979));
#4053=CARTESIAN_POINT('',(91.,-70.0000000000105,-34.9999999999979));
#4054=CARTESIAN_POINT('Origin',(91.,69.2928932188029,-34.2928932188113));
#4055=CARTESIAN_POINT('',(90.,84.5857864376164,-18.9999999999979));
#4056=CARTESIAN_POINT('',(90.,88.9999999999895,-14.5857864376248));
#4057=CARTESIAN_POINT('',(90.,69.2928932188029,-34.2928932188113));
#4058=CARTESIAN_POINT('',(91.,89.9999999999895,-14.9999999999979));
#4059=CARTESIAN_POINT('Origin',(91.,88.9999999999895,-14.5857864376248));
#4060=CARTESIAN_POINT('',(91.,84.9999999999895,-19.9999999999979));
#4061=CARTESIAN_POINT('',(91.,69.9999999999895,-34.9999999999979));
#4062=CARTESIAN_POINT('Origin',(91.,84.5857864376164,-18.9999999999979));
#4063=CARTESIAN_POINT('Origin',(91.,88.9999999999895,-9.99999999999789));
#4064=CARTESIAN_POINT('',(91.,89.9999999999895,15.0000000000021));
#4065=CARTESIAN_POINT('',(91.,89.9999999999895,-9.99999999999789));
#4066=CARTESIAN_POINT('',(90.,88.9999999999895,14.585786437629));
#4067=CARTESIAN_POINT('',(90.,88.9999999999895,-9.99999999999789));
#4068=CARTESIAN_POINT('Origin',(91.,88.9999999999895,14.585786437629));
#4069=CARTESIAN_POINT('Origin',(91.,-45.0000000000105,-18.9999999999979));
#4070=CARTESIAN_POINT('',(90.,-45.0000000000105,-18.9999999999979));
#4071=CARTESIAN_POINT('',(91.,-45.0000000000105,-19.9999999999979));
#4072=CARTESIAN_POINT('Origin',(91.,69.2928932188029,34.2928932188156));
#4073=CARTESIAN_POINT('',(91.,84.9999999999895,20.0000000000021));
#4074=CARTESIAN_POINT('',(91.,69.9999999999895,35.0000000000021));
#4075=CARTESIAN_POINT('',(90.,84.5857864376164,19.0000000000021));
#4076=CARTESIAN_POINT('',(90.,69.2928932188029,34.2928932188156));
#4077=CARTESIAN_POINT('Origin',(91.,84.5857864376164,19.0000000000021));
#4078=CARTESIAN_POINT('Origin',(91.,44.9999999999895,19.0000000000021));
#4079=CARTESIAN_POINT('',(91.,44.9999999999895,20.0000000000021));
#4080=CARTESIAN_POINT('',(90.,44.9999999999895,19.0000000000021));
#4081=CARTESIAN_POINT('Origin',(110.,-90.0000000000105,20.0000000000021));
#4082=CARTESIAN_POINT('',(110.,-90.0000000000105,-14.9999999999979));
#4083=CARTESIAN_POINT('',(110.,-90.0000000000105,-14.9999999999979));
#4084=CARTESIAN_POINT('',(110.,-90.0000000000105,15.0000000000021));
#4085=CARTESIAN_POINT('',(110.,-90.0000000000105,20.0000000000021));
#4086=CARTESIAN_POINT('',(110.,-90.0000000000105,15.0000000000021));
#4087=CARTESIAN_POINT('Origin',(110.,-87.5000000000105,-17.4999999999979));
#4088=CARTESIAN_POINT('',(110.,-85.0000000000105,-19.9999999999979));
#4089=CARTESIAN_POINT('',(110.,-85.0000000000105,-19.9999999999979));
#4090=CARTESIAN_POINT('',(110.,-70.0000000000105,-34.9999999999979));
#4091=CARTESIAN_POINT('Origin',(110.,-90.0000000000105,-19.9999999999979));
#4092=CARTESIAN_POINT('',(110.,84.9999999999895,-19.9999999999979));
#4093=CARTESIAN_POINT('',(110.,84.9999999999895,-19.9999999999979));
#4094=CARTESIAN_POINT('',(110.,-90.0000000000105,-19.9999999999979));
#4095=CARTESIAN_POINT('Origin',(110.,87.4999999999895,-17.4999999999979));
#4096=CARTESIAN_POINT('',(110.,89.9999999999895,-14.9999999999979));
#4097=CARTESIAN_POINT('',(110.,89.9999999999895,-14.9999999999979));
#4098=CARTESIAN_POINT('',(110.,69.9999999999895,-34.9999999999979));
#4099=CARTESIAN_POINT('Origin',(90.,-1.05160324892495E-11,2.1138646388863E-12));
#4100=CARTESIAN_POINT('Origin',(110.,87.4999999999895,17.5000000000021));
#4101=CARTESIAN_POINT('',(110.,84.9999999999895,20.0000000000021));
#4102=CARTESIAN_POINT('',(110.,84.9999999999895,20.0000000000021));
#4103=CARTESIAN_POINT('',(110.,89.9999999999895,15.0000000000021));
#4104=CARTESIAN_POINT('',(110.,69.9999999999895,35.0000000000021));
#4105=CARTESIAN_POINT('',(110.,89.9999999999895,15.0000000000021));
#4106=CARTESIAN_POINT('Origin',(110.,89.9999999999895,-19.9999999999979));
#4107=CARTESIAN_POINT('',(110.,89.9999999999895,-19.9999999999979));
#4108=CARTESIAN_POINT('Origin',(110.,-87.5000000000105,17.5000000000021));
#4109=CARTESIAN_POINT('',(110.,-85.0000000000105,20.0000000000021));
#4110=CARTESIAN_POINT('',(110.,-70.0000000000105,35.0000000000021));
#4111=CARTESIAN_POINT('',(110.,-85.0000000000105,20.0000000000021));
#4112=CARTESIAN_POINT('Origin',(110.,89.9999999999895,20.0000000000021));
#4113=CARTESIAN_POINT('',(110.,89.9999999999895,20.0000000000021));
#4114=CARTESIAN_POINT('Origin',(110.,-1.05160324892495E-11,2.11275441586167E-12));
#4115=CARTESIAN_POINT('',(0.,0.,0.));
#4116=CARTESIAN_POINT('Origin',(89.,-70.542893218824,33.0428932188156));
#4117=CARTESIAN_POINT('',(90.,-89.0000000000105,14.585786437629));
#4118=CARTESIAN_POINT('',(90.,-84.5857864376374,19.0000000000021));
#4119=CARTESIAN_POINT('',(90.,-70.542893218824,33.0428932188156));
#4120=CARTESIAN_POINT('',(89.,-85.0000000000105,20.0000000000021));
#4121=CARTESIAN_POINT('Origin',(89.,-84.5857864376374,19.0000000000021));
#4122=CARTESIAN_POINT('',(89.,-90.0000000000105,15.0000000000021));
#4123=CARTESIAN_POINT('',(89.,-71.2500000000105,33.7500000000021));
#4124=CARTESIAN_POINT('Origin',(89.,-89.0000000000105,14.585786437629));
#4125=CARTESIAN_POINT('Origin',(89.,-42.5000000000105,19.0000000000021));
#4126=CARTESIAN_POINT('',(90.,84.5857864376164,19.0000000000021));
#4127=CARTESIAN_POINT('',(90.,-42.5000000000105,19.0000000000021));
#4128=CARTESIAN_POINT('',(89.,84.9999999999895,20.0000000000021));
#4129=CARTESIAN_POINT('Origin',(89.,84.5857864376164,19.0000000000021));
#4130=CARTESIAN_POINT('',(89.,-42.5000000000105,20.0000000000021));
#4131=CARTESIAN_POINT('Origin',(89.,88.9999999999895,7.50000000000211));
#4132=CARTESIAN_POINT('',(89.,89.9999999999895,-14.9999999999979));
#4133=CARTESIAN_POINT('',(89.,89.9999999999895,15.0000000000021));
#4134=CARTESIAN_POINT('',(89.,89.9999999999895,7.50000000000211));
#4135=CARTESIAN_POINT('',(90.,88.9999999999895,14.585786437629));
#4136=CARTESIAN_POINT('Origin',(89.,88.9999999999895,14.585786437629));
#4137=CARTESIAN_POINT('',(90.,88.9999999999895,-14.5857864376248));
#4138=CARTESIAN_POINT('',(90.,88.9999999999895,7.50000000000211));
#4139=CARTESIAN_POINT('Origin',(89.,88.9999999999895,-14.5857864376248));
#4140=CARTESIAN_POINT('Origin',(89.,68.042893218803,35.5428932188156));
#4141=CARTESIAN_POINT('',(90.,68.042893218803,35.5428932188156));
#4142=CARTESIAN_POINT('',(89.,68.7499999999895,36.2500000000021));
#4143=CARTESIAN_POINT('Origin',(89.,70.5428932188029,-33.0428932188113));
#4144=CARTESIAN_POINT('',(89.,84.9999999999895,-19.9999999999979));
#4145=CARTESIAN_POINT('',(89.,71.2499999999895,-33.7499999999979));
#4146=CARTESIAN_POINT('',(90.,84.5857864376164,-18.9999999999979));
#4147=CARTESIAN_POINT('',(90.,70.5428932188029,-33.0428932188113));
#4148=CARTESIAN_POINT('Origin',(89.,84.5857864376164,-18.9999999999979));
#4149=CARTESIAN_POINT('Origin',(89.,42.4999999999895,-18.9999999999979));
#4150=CARTESIAN_POINT('',(89.,-85.0000000000105,-19.9999999999979));
#4151=CARTESIAN_POINT('',(89.,42.4999999999895,-19.9999999999979));
#4152=CARTESIAN_POINT('',(90.,-84.5857864376374,-18.9999999999979));
#4153=CARTESIAN_POINT('',(90.,42.4999999999895,-18.9999999999979));
#4154=CARTESIAN_POINT('Origin',(89.,-84.5857864376374,-18.9999999999979));
#4155=CARTESIAN_POINT('Origin',(89.,-68.042893218824,-35.5428932188113));
#4156=CARTESIAN_POINT('',(89.,-90.0000000000105,-14.9999999999979));
#4157=CARTESIAN_POINT('',(89.,-68.7500000000105,-36.2499999999979));
#4158=CARTESIAN_POINT('',(90.,-89.0000000000105,-14.5857864376248));
#4159=CARTESIAN_POINT('',(90.,-68.042893218824,-35.5428932188113));
#4160=CARTESIAN_POINT('Origin',(89.,-89.0000000000105,-14.5857864376248));
#4161=CARTESIAN_POINT('Origin',(89.,-89.0000000000105,-7.49999999999789));
#4162=CARTESIAN_POINT('',(89.,-90.0000000000105,-7.49999999999789));
#4163=CARTESIAN_POINT('',(90.,-89.0000000000105,-7.49999999999789));
#4164=CARTESIAN_POINT('Origin',(90.,-90.0000000000105,15.0000000000021));
#4165=CARTESIAN_POINT('',(70.,-85.0000000000105,20.0000000000021));
#4166=CARTESIAN_POINT('',(90.,-85.0000000000105,20.0000000000021));
#4167=CARTESIAN_POINT('',(70.,-90.0000000000105,15.0000000000021));
#4168=CARTESIAN_POINT('',(70.,-90.0000000000105,15.0000000000021));
#4169=CARTESIAN_POINT('',(90.,-90.0000000000105,15.0000000000021));
#4170=CARTESIAN_POINT('Origin',(90.,-85.0000000000105,20.0000000000021));
#4171=CARTESIAN_POINT('',(85.,84.9999999999895,20.0000000000021));
#4172=CARTESIAN_POINT('',(90.,84.9999999999895,20.0000000000021));
#4173=CARTESIAN_POINT('',(85.,29.9999999999895,20.0000000000021));
#4174=CARTESIAN_POINT('',(85.,-12.5000000000105,20.0000000000021));
#4175=CARTESIAN_POINT('',(70.,29.9999999999895,20.0000000000021));
#4176=CARTESIAN_POINT('',(80.,29.9999999999895,20.0000000000021));
#4177=CARTESIAN_POINT('',(70.,-85.0000000000105,20.0000000000021));
#4178=CARTESIAN_POINT('Origin',(90.,84.9999999999895,20.0000000000021));
#4179=CARTESIAN_POINT('',(85.,89.9999999999895,15.0000000000021));
#4180=CARTESIAN_POINT('',(90.,89.9999999999895,15.0000000000021));
#4181=CARTESIAN_POINT('',(85.,83.7499999999895,21.2500000000021));
#4182=CARTESIAN_POINT('Origin',(90.,89.9999999999895,15.0000000000021));
#4183=CARTESIAN_POINT('',(85.,89.9999999999895,-14.9999999999979));
#4184=CARTESIAN_POINT('',(90.,89.9999999999895,-14.9999999999979));
#4185=CARTESIAN_POINT('',(85.,89.9999999999895,7.50000000000211));
#4186=CARTESIAN_POINT('Origin',(90.,-1.05160324892495E-11,2.11275441586167E-12));
#4187=CARTESIAN_POINT('Origin',(70.,29.9999999999895,20.0000000000021));
#4188=CARTESIAN_POINT('',(70.,29.9999999999895,-19.9999999999979));
#4189=CARTESIAN_POINT('',(70.,29.9999999999895,10.0000000000021));
#4190=CARTESIAN_POINT('',(85.,29.9999999999895,-19.9999999999979));
#4191=CARTESIAN_POINT('',(85.,29.9999999999895,20.0000000000021));
#4192=CARTESIAN_POINT('',(80.,29.9999999999895,-19.9999999999979));
#4193=CARTESIAN_POINT('Origin',(85.,59.9999999999895,2.1138646388863E-12));
#4194=CARTESIAN_POINT('',(85.,84.9999999999895,-19.9999999999979));
#4195=CARTESIAN_POINT('',(85.,86.2499999999895,-18.7499999999979));
#4196=CARTESIAN_POINT('',(85.,72.4999999999895,-19.9999999999979));
#4197=CARTESIAN_POINT('Origin',(90.,89.9999999999895,-14.9999999999979));
#4198=CARTESIAN_POINT('',(90.,84.9999999999895,-19.9999999999979));
#4199=CARTESIAN_POINT('Origin',(90.,-90.0000000000105,-14.9999999999979));
#4200=CARTESIAN_POINT('',(70.,-90.0000000000105,-14.9999999999979));
#4201=CARTESIAN_POINT('',(70.,-90.0000000000105,-14.9999999999979));
#4202=CARTESIAN_POINT('',(90.,-90.0000000000105,-14.9999999999979));
#4203=CARTESIAN_POINT('Origin',(90.,-85.0000000000105,-19.9999999999979));
#4204=CARTESIAN_POINT('',(70.,-85.0000000000105,-19.9999999999979));
#4205=CARTESIAN_POINT('',(70.,-85.0000000000105,-19.9999999999979));
#4206=CARTESIAN_POINT('',(90.,-85.0000000000105,-19.9999999999979));
#4207=CARTESIAN_POINT('Origin',(90.,84.9999999999895,-19.9999999999979));
#4208=CARTESIAN_POINT('',(70.,84.9999999999895,-19.9999999999979));
#4209=CARTESIAN_POINT('Origin',(70.,-1.05160324892495E-11,2.11164419283705E-12));
#4210=CARTESIAN_POINT('',(0.,0.,0.));
#4211=CARTESIAN_POINT('Origin',(70.,-30.0000000000105,7.00000000000211));
#4212=CARTESIAN_POINT('',(60.,-23.0000000000105,7.00000000000211));
#4213=CARTESIAN_POINT('Origin',(60.,-30.0000000000105,7.00000000000211));
#4214=CARTESIAN_POINT('',(69.,-23.0000000000105,7.00000000000211));
#4215=CARTESIAN_POINT('',(70.,-23.0000000000105,7.00000000000211));
#4216=CARTESIAN_POINT('Origin',(69.,-30.0000000000105,7.00000000000211));
#4217=CARTESIAN_POINT('Origin',(70.,-30.0000000000105,7.00000000000211));
#4218=CARTESIAN_POINT('',(60.,-24.0000000000105,7.00000000000211));
#4219=CARTESIAN_POINT('Origin',(60.,-30.0000000000105,7.00000000000211));
#4220=CARTESIAN_POINT('',(70.,-24.0000000000105,7.00000000000211));
#4221=CARTESIAN_POINT('',(70.,-24.0000000000105,7.00000000000211));
#4222=CARTESIAN_POINT('Origin',(70.,-30.0000000000105,7.00000000000211));
#4223=CARTESIAN_POINT('Origin',(60.,-30.0000000000105,7.00000000000211));
#4224=CARTESIAN_POINT('Origin',(70.,-30.0000000000105,7.00000000000211));
#4225=CARTESIAN_POINT('',(69.,-19.0000000000105,7.00000000000211));
#4226=CARTESIAN_POINT('Origin',(69.,-30.0000000000105,7.00000000000211));
#4227=CARTESIAN_POINT('',(70.,-19.0000000000105,7.00000000000211));
#4228=CARTESIAN_POINT('',(70.,-19.0000000000105,7.00000000000211));
#4229=CARTESIAN_POINT('Origin',(70.,-30.0000000000105,7.00000000000211));
#4230=CARTESIAN_POINT('Origin',(69.,-30.0000000000105,7.00000000000211));
#4231=CARTESIAN_POINT('Origin',(70.,-30.0000000000105,7.00000000000211));
#4232=CARTESIAN_POINT('',(0.,0.,0.));
#4233=CARTESIAN_POINT('Origin',(70.,-60.0000000000105,-5.99999999999788));
#4234=CARTESIAN_POINT('',(-90.,-60.0000000000105,-5.99999999999788));
#4235=CARTESIAN_POINT('',(70.,-60.0000000000105,-5.99999999999788));
#4236=CARTESIAN_POINT('',(70.,-60.0000000000105,-5.99999999999788));
#4237=CARTESIAN_POINT('',(-90.,-60.0000000000105,4.00000000000212));
#4238=CARTESIAN_POINT('',(-90.,-60.0000000000105,-5.99999999999788));
#4239=CARTESIAN_POINT('',(70.,-60.0000000000105,4.00000000000212));
#4240=CARTESIAN_POINT('',(70.,-60.0000000000105,4.00000000000212));
#4241=CARTESIAN_POINT('',(70.,-60.0000000000105,-5.99999999999788));
#4242=CARTESIAN_POINT('Origin',(-10.,-75.0000000000105,4.00000000000212));
#4243=CARTESIAN_POINT('',(-90.,-90.0000000000105,4.00000000000212));
#4244=CARTESIAN_POINT('',(-90.,-60.0000000000105,4.00000000000212));
#4245=CARTESIAN_POINT('',(70.,-90.0000000000105,4.00000000000212));
#4246=CARTESIAN_POINT('',(-90.,-90.0000000000105,4.00000000000212));
#4247=CARTESIAN_POINT('',(70.,-90.0000000000105,4.00000000000212));
#4248=CARTESIAN_POINT('Origin',(70.,-90.0000000000105,-5.99999999999788));
#4249=CARTESIAN_POINT('',(70.,-1.05160324892495E-11,-5.99999999999788));
#4250=CARTESIAN_POINT('',(70.,-90.0000000000105,-5.99999999999788));
#4251=CARTESIAN_POINT('',(-90.,-1.05160324892495E-11,-5.99999999999788));
#4252=CARTESIAN_POINT('',(-10.,-1.05160324892495E-11,-5.99999999999788));
#4253=CARTESIAN_POINT('',(-90.,-90.0000000000105,-5.99999999999788));
#4254=CARTESIAN_POINT('Origin',(-90.,-1.05160324892495E-11,-5.99999999999788));
#4255=CARTESIAN_POINT('',(70.,-1.05160324892495E-11,4.00000000000212));
#4256=CARTESIAN_POINT('',(70.,-1.05160324892495E-11,-5.99999999999788));
#4257=CARTESIAN_POINT('',(-90.,-1.05160324892495E-11,4.00000000000212));
#4258=CARTESIAN_POINT('',(70.,-1.05160324892495E-11,4.00000000000212));
#4259=CARTESIAN_POINT('',(-90.,-1.05160324892495E-11,-5.99999999999788));
#4260=CARTESIAN_POINT('Origin',(-10.,14.9999999999895,4.00000000000212));
#4261=CARTESIAN_POINT('',(70.,29.9999999999895,4.00000000000212));
#4262=CARTESIAN_POINT('',(70.,29.9999999999895,4.00000000000212));
#4263=CARTESIAN_POINT('',(-90.,29.9999999999895,4.00000000000212));
#4264=CARTESIAN_POINT('',(-90.,29.9999999999895,4.00000000000212));
#4265=CARTESIAN_POINT('',(-90.,-1.05160324892495E-11,4.00000000000212));
#4266=CARTESIAN_POINT('Origin',(70.,-90.0000000000105,-14.9999999999979));
#4267=CARTESIAN_POINT('',(70.,-90.0000000000105,-14.9999999999979));
#4268=CARTESIAN_POINT('',(70.,-90.0000000000105,-19.9999999999979));
#4269=CARTESIAN_POINT('',(-90.,-90.0000000000105,-14.9999999999979));
#4270=CARTESIAN_POINT('',(-90.,-90.0000000000105,-19.9999999999979));
#4271=CARTESIAN_POINT('',(70.,-90.0000000000105,-14.9999999999979));
#4272=CARTESIAN_POINT('Origin',(70.,-85.0000000000105,-19.9999999999979));
#4273=CARTESIAN_POINT('',(70.,-85.0000000000105,-19.9999999999979));
#4274=CARTESIAN_POINT('',(70.,-85.0000000000105,-19.9999999999979));
#4275=CARTESIAN_POINT('',(-90.,-85.0000000000105,-19.9999999999979));
#4276=CARTESIAN_POINT('',(-90.,-85.0000000000105,-19.9999999999979));
#4277=CARTESIAN_POINT('',(70.,-85.0000000000105,-19.9999999999979));
#4278=CARTESIAN_POINT('Origin',(70.,29.9999999999895,-19.9999999999979));
#4279=CARTESIAN_POINT('',(70.,29.9999999999895,-19.9999999999979));
#4280=CARTESIAN_POINT('',(70.,29.9999999999895,-19.9999999999979));
#4281=CARTESIAN_POINT('',(-90.,29.9999999999895,-19.9999999999979));
#4282=CARTESIAN_POINT('',(-90.,29.9999999999895,-19.9999999999979));
#4283=CARTESIAN_POINT('',(70.,29.9999999999895,-19.9999999999979));
#4284=CARTESIAN_POINT('Origin',(70.,29.9999999999895,-5.99999999999788));
#4285=CARTESIAN_POINT('',(70.,29.9999999999895,-5.99999999999788));
#4286=CARTESIAN_POINT('',(-90.,29.9999999999895,-5.99999999999788));
#4287=CARTESIAN_POINT('Origin',(-90.,-30.0000000000105,-12.9999999999979));
#4288=CARTESIAN_POINT('Origin',(70.,-30.0000000000105,-12.9999999999979));
#4289=CARTESIAN_POINT('',(0.,0.,0.));
#4290=CARTESIAN_POINT('Origin',(-34.3120542422792,-30.0000000000105,20.0000000000021));
#4291=CARTESIAN_POINT('',(-29.3120542422792,-30.0000000000105,20.0000000000021));
#4292=CARTESIAN_POINT('Origin',(-34.3120542422792,-30.0000000000105,20.0000000000021));
#4293=CARTESIAN_POINT('',(-29.3120542422792,-30.0000000000105,13.0000000000021));
#4294=CARTESIAN_POINT('',(-29.3120542422792,-30.0000000000105,20.0000000000021));
#4295=CARTESIAN_POINT('',(-34.3120542422792,-35.0000000000105,10.3166247903575));
#4296=CARTESIAN_POINT('Ctrl Pts',(-34.3120542422792,-35.0000000000105,10.3166247903575));
#4297=CARTESIAN_POINT('Ctrl Pts',(-33.9649654150723,-35.0000000000105,10.3166247903575));
#4298=CARTESIAN_POINT('Ctrl Pts',(-33.6249191325797,-34.9638640057048,10.372517968392));
#4299=CARTESIAN_POINT('Ctrl Pts',(-32.9692326416159,-34.8279323440191,10.564392312562));
#4300=CARTESIAN_POINT('Ctrl Pts',(-32.6532784827973,-34.7281094760039,10.6992796672134));
#4301=CARTESIAN_POINT('Ctrl Pts',(-31.7522928141166,-34.3444039514126,11.1575129861594));
#4302=CARTESIAN_POINT('Ctrl Pts',(-31.2127810222979,-33.9717945918947,11.5295040511826));
#4303=CARTESIAN_POINT('Ctrl Pts',(-30.3579885926001,-33.1170021621969,12.1529255036342));
#4304=CARTESIAN_POINT('Ctrl Pts',(-29.9764667659311,-32.5780383625098,12.4565421384626));
#4305=CARTESIAN_POINT('Ctrl Pts',(-29.4527956614068,-31.3532217388044,12.8812351576426));
#4306=CARTESIAN_POINT('Ctrl Pts',(-29.3120542422792,-30.6659673757733,13.0000000000021));
#4307=CARTESIAN_POINT('Ctrl Pts',(-29.3120542422792,-30.0000000000105,13.0000000000021));
#4308=CARTESIAN_POINT('Ctrl Pts',(-29.3120542422792,-30.0000000000105,13.0000000000021));
#4309=CARTESIAN_POINT('Ctrl Pts',(-29.3120542422792,-29.3340326242477,13.0000000000021));
#4310=CARTESIAN_POINT('Ctrl Pts',(-29.4527956614068,-28.6467782612167,12.8812351576426));
#4311=CARTESIAN_POINT('Ctrl Pts',(-29.9764667659311,-27.4219616375112,12.4565421384626));
#4312=CARTESIAN_POINT('Ctrl Pts',(-30.3579885926001,-26.8829978378241,12.1529255036342));
#4313=CARTESIAN_POINT('Ctrl Pts',(-31.2127810222979,-26.0282054081263,11.5295040511826));
#4314=CARTESIAN_POINT('Ctrl Pts',(-31.7522928141166,-25.6555960486084,11.1575129861594));
#4315=CARTESIAN_POINT('Ctrl Pts',(-32.6532784827973,-25.2718905240171,10.6992796672134));
#4316=CARTESIAN_POINT('Ctrl Pts',(-32.9692326416159,-25.172067656002,10.564392312562));
#4317=CARTESIAN_POINT('Ctrl Pts',(-33.6249191325797,-25.0361359943163,10.372517968392));
#4318=CARTESIAN_POINT('Ctrl Pts',(-33.9649654150723,-25.0000000000105,10.3166247903575));
#4319=CARTESIAN_POINT('Ctrl Pts',(-34.6591430694861,-25.0000000000105,10.3166247903575));
#4320=CARTESIAN_POINT('Ctrl Pts',(-34.9991893519787,-25.0361359943163,10.372517968392));
#4321=CARTESIAN_POINT('Ctrl Pts',(-35.6548758429425,-25.172067656002,10.564392312562));
#4322=CARTESIAN_POINT('Ctrl Pts',(-35.9708300017611,-25.2718905240171,10.6992796672134));
#4323=CARTESIAN_POINT('Ctrl Pts',(-36.8718156704418,-25.6555960486084,11.1575129861594));
#4324=CARTESIAN_POINT('Ctrl Pts',(-37.4113274622605,-26.0282054081263,11.5295040511826));
#4325=CARTESIAN_POINT('Ctrl Pts',(-38.2661198919583,-26.8829978378241,12.1529255036342));
#4326=CARTESIAN_POINT('Ctrl Pts',(-38.6476417186273,-27.4219616375112,12.4565421384626));
#4327=CARTESIAN_POINT('Ctrl Pts',(-39.1713128231516,-28.6467782612166,12.8812351576426));
#4328=CARTESIAN_POINT('Ctrl Pts',(-39.3120542422792,-29.3340326242477,13.0000000000021));
#4329=CARTESIAN_POINT('Ctrl Pts',(-39.3120542422792,-30.6659673757733,13.0000000000021));
#4330=CARTESIAN_POINT('Ctrl Pts',(-39.1713128231516,-31.3532217388044,12.8812351576426));
#4331=CARTESIAN_POINT('Ctrl Pts',(-38.6476417186273,-32.5780383625099,12.4565421384626));
#4332=CARTESIAN_POINT('Ctrl Pts',(-38.2661198919583,-33.1170021621969,12.1529255036342));
#4333=CARTESIAN_POINT('Ctrl Pts',(-37.4113274622605,-33.9717945918947,11.5295040511826));
#4334=CARTESIAN_POINT('Ctrl Pts',(-36.8718156704418,-34.3444039514126,11.1575129861594));
#4335=CARTESIAN_POINT('Ctrl Pts',(-35.9708300017611,-34.7281094760039,10.6992796672134));
#4336=CARTESIAN_POINT('Ctrl Pts',(-35.6548758429425,-34.8279323440191,10.564392312562));
#4337=CARTESIAN_POINT('Ctrl Pts',(-34.9991893519787,-34.9638640057048,10.372517968392));
#4338=CARTESIAN_POINT('Ctrl Pts',(-34.6591430694861,-35.0000000000105,10.3166247903575));
#4339=CARTESIAN_POINT('Ctrl Pts',(-34.3120542422792,-35.0000000000105,10.3166247903575));
#4340=CARTESIAN_POINT('Origin',(-34.3120542422792,-30.0000000000105,20.0000000000021));
#4341=CARTESIAN_POINT('',(-34.3120542422792,-35.0000000000105,3.68337520964672));
#4342=CARTESIAN_POINT('',(-29.3120542422792,-30.0000000000105,1.00000000000212));
#4343=CARTESIAN_POINT('Ctrl Pts',(-34.3120542422792,-35.0000000000105,3.68337520964672));
#4344=CARTESIAN_POINT('Ctrl Pts',(-34.6591430694861,-35.0000000000105,3.68337520964672));
#4345=CARTESIAN_POINT('Ctrl Pts',(-34.9991893519787,-34.9638640057048,3.62748203161225));
#4346=CARTESIAN_POINT('Ctrl Pts',(-35.6548758429425,-34.8279323440191,3.43560768744221));
#4347=CARTESIAN_POINT('Ctrl Pts',(-35.9708300017611,-34.7281094760039,3.30072033279082));
#4348=CARTESIAN_POINT('Ctrl Pts',(-36.8718156704418,-34.3444039514126,2.84248701384487));
#4349=CARTESIAN_POINT('Ctrl Pts',(-37.4113274622605,-33.9717945918947,2.47049594882166));
#4350=CARTESIAN_POINT('Ctrl Pts',(-38.2661198919583,-33.1170021621969,1.84707449637));
#4351=CARTESIAN_POINT('Ctrl Pts',(-38.6476417186273,-32.5780383625099,1.54345786154165));
#4352=CARTESIAN_POINT('Ctrl Pts',(-39.1713128231516,-31.3532217388044,1.1187648423616));
#4353=CARTESIAN_POINT('Ctrl Pts',(-39.3120542422792,-30.6659673757733,1.00000000000212));
#4354=CARTESIAN_POINT('Ctrl Pts',(-39.3120542422792,-29.3340326242477,1.00000000000212));
#4355=CARTESIAN_POINT('Ctrl Pts',(-39.1713128231516,-28.6467782612166,1.1187648423616));
#4356=CARTESIAN_POINT('Ctrl Pts',(-38.6476417186273,-27.4219616375112,1.54345786154166));
#4357=CARTESIAN_POINT('Ctrl Pts',(-38.2661198919583,-26.8829978378241,1.84707449637));
#4358=CARTESIAN_POINT('Ctrl Pts',(-37.4113274622605,-26.0282054081263,2.47049594882166));
#4359=CARTESIAN_POINT('Ctrl Pts',(-36.8718156704418,-25.6555960486084,2.84248701384487));
#4360=CARTESIAN_POINT('Ctrl Pts',(-35.9708300017611,-25.2718905240171,3.30072033279082));
#4361=CARTESIAN_POINT('Ctrl Pts',(-35.6548758429425,-25.172067656002,3.43560768744221));
#4362=CARTESIAN_POINT('Ctrl Pts',(-34.9991893519787,-25.0361359943163,3.62748203161225));
#4363=CARTESIAN_POINT('Ctrl Pts',(-34.6591430694861,-25.0000000000105,3.68337520964672));
#4364=CARTESIAN_POINT('Ctrl Pts',(-33.9649654150723,-25.0000000000105,3.68337520964672));
#4365=CARTESIAN_POINT('Ctrl Pts',(-33.6249191325797,-25.0361359943163,3.62748203161224));
#4366=CARTESIAN_POINT('Ctrl Pts',(-32.9692326416159,-25.172067656002,3.43560768744219));
#4367=CARTESIAN_POINT('Ctrl Pts',(-32.6532784827973,-25.2718905240171,3.30072033279081));
#4368=CARTESIAN_POINT('Ctrl Pts',(-31.7522928141166,-25.6555960486084,2.84248701384486));
#4369=CARTESIAN_POINT('Ctrl Pts',(-31.2127810222979,-26.0282054081263,2.47049594882166));
#4370=CARTESIAN_POINT('Ctrl Pts',(-30.3579885926001,-26.8829978378241,1.84707449636999));
#4371=CARTESIAN_POINT('Ctrl Pts',(-29.9764667659311,-27.4219616375112,1.54345786154165));
#4372=CARTESIAN_POINT('Ctrl Pts',(-29.4527956614068,-28.6467782612166,1.1187648423616));
#4373=CARTESIAN_POINT('Ctrl Pts',(-29.3120542422792,-29.3340326242477,1.00000000000212));
#4374=CARTESIAN_POINT('Ctrl Pts',(-29.3120542422792,-30.0000000000105,1.00000000000212));
#4375=CARTESIAN_POINT('Ctrl Pts',(-29.3120542422792,-30.0000000000105,1.00000000000212));
#4376=CARTESIAN_POINT('Ctrl Pts',(-29.3120542422792,-30.6659673757733,1.00000000000212));
#4377=CARTESIAN_POINT('Ctrl Pts',(-29.4527956614068,-31.3532217388044,1.1187648423616));
#4378=CARTESIAN_POINT('Ctrl Pts',(-29.9764667659311,-32.5780383625098,1.54345786154165));
#4379=CARTESIAN_POINT('Ctrl Pts',(-30.3579885926001,-33.1170021621969,1.84707449636999));
#4380=CARTESIAN_POINT('Ctrl Pts',(-31.2127810222979,-33.9717945918947,2.47049594882166));
#4381=CARTESIAN_POINT('Ctrl Pts',(-31.7522928141166,-34.3444039514126,2.84248701384486));
#4382=CARTESIAN_POINT('Ctrl Pts',(-32.6532784827973,-34.7281094760039,3.30072033279081));
#4383=CARTESIAN_POINT('Ctrl Pts',(-32.9692326416159,-34.8279323440191,3.43560768744219));
#4384=CARTESIAN_POINT('Ctrl Pts',(-33.6249191325797,-34.9638640057048,3.62748203161224));
#4385=CARTESIAN_POINT('Ctrl Pts',(-33.9649654150723,-35.0000000000105,3.68337520964672));
#4386=CARTESIAN_POINT('Ctrl Pts',(-34.3120542422792,-35.0000000000105,3.68337520964672));
#4387=CARTESIAN_POINT('',(-29.3120542422792,-30.0000000000105,-5.99999999999788));
#4388=CARTESIAN_POINT('',(-29.3120542422792,-30.0000000000105,20.0000000000021));
#4389=CARTESIAN_POINT('Origin',(-34.3120542422792,-30.0000000000105,-5.99999999999788));
#4390=CARTESIAN_POINT('Origin',(-34.3120542422792,14.9999999999895,20.0000000000021));
#4391=CARTESIAN_POINT('',(-29.3120542422792,14.9999999999895,20.0000000000021));
#4392=CARTESIAN_POINT('Origin',(-34.3120542422792,14.9999999999895,20.0000000000021));
#4393=CARTESIAN_POINT('',(-29.3120542422792,14.9999999999895,14.0000000000021));
#4394=CARTESIAN_POINT('',(-29.3120542422792,14.9999999999895,20.0000000000021));
#4395=CARTESIAN_POINT('Origin',(-34.3120542422792,14.9999999999895,14.0000000000021));
#4396=CARTESIAN_POINT('Origin',(-14.3120542422792,-75.0000000000105,20.0000000000021));
#4397=CARTESIAN_POINT('',(-9.3120542422792,-75.0000000000105,20.0000000000021));
#4398=CARTESIAN_POINT('Origin',(-14.3120542422792,-75.0000000000105,20.0000000000021));
#4399=CARTESIAN_POINT('',(-9.3120542422792,-75.0000000000105,14.0000000000021));
#4400=CARTESIAN_POINT('',(-9.3120542422792,-75.0000000000105,20.0000000000021));
#4401=CARTESIAN_POINT('Origin',(-14.3120542422792,-75.0000000000105,14.0000000000021));
#4402=CARTESIAN_POINT('Origin',(10.6879457577208,-30.0000000000105,20.0000000000021));
#4403=CARTESIAN_POINT('',(15.6879457577208,-30.0000000000105,20.0000000000021));
#4404=CARTESIAN_POINT('Origin',(10.6879457577208,-30.0000000000105,20.0000000000021));
#4405=CARTESIAN_POINT('',(15.6879457577208,-30.0000000000105,13.0000000000021));
#4406=CARTESIAN_POINT('',(15.6879457577208,-30.0000000000105,20.0000000000021));
#4407=CARTESIAN_POINT('',(10.6879457577208,-35.0000000000105,10.3166247903575));
#4408=CARTESIAN_POINT('Ctrl Pts',(10.6879457577208,-35.0000000000105,10.3166247903575));
#4409=CARTESIAN_POINT('Ctrl Pts',(11.0350345849277,-35.0000000000105,10.3166247903575));
#4410=CARTESIAN_POINT('Ctrl Pts',(11.3750808674203,-34.9638640057048,10.372517968392));
#4411=CARTESIAN_POINT('Ctrl Pts',(12.0307673583841,-34.8279323440191,10.564392312562));
#4412=CARTESIAN_POINT('Ctrl Pts',(12.3467215172027,-34.7281094760039,10.6992796672134));
#4413=CARTESIAN_POINT('Ctrl Pts',(13.2477071858834,-34.3444039514126,11.1575129861594));
#4414=CARTESIAN_POINT('Ctrl Pts',(13.7872189777021,-33.9717945918947,11.5295040511826));
#4415=CARTESIAN_POINT('Ctrl Pts',(14.6420114073999,-33.1170021621969,12.1529255036342));
#4416=CARTESIAN_POINT('Ctrl Pts',(15.0235332340689,-32.5780383625099,12.4565421384626));
#4417=CARTESIAN_POINT('Ctrl Pts',(15.5472043385932,-31.3532217388044,12.8812351576426));
#4418=CARTESIAN_POINT('Ctrl Pts',(15.6879457577208,-30.6659673757733,13.0000000000021));
#4419=CARTESIAN_POINT('Ctrl Pts',(15.6879457577208,-30.0000000000105,13.0000000000021));
#4420=CARTESIAN_POINT('Ctrl Pts',(15.6879457577208,-30.0000000000105,13.0000000000021));
#4421=CARTESIAN_POINT('Ctrl Pts',(15.6879457577208,-29.3340326242477,13.0000000000021));
#4422=CARTESIAN_POINT('Ctrl Pts',(15.5472043385932,-28.6467782612166,12.8812351576426));
#4423=CARTESIAN_POINT('Ctrl Pts',(15.0235332340689,-27.4219616375112,12.4565421384626));
#4424=CARTESIAN_POINT('Ctrl Pts',(14.6420114073999,-26.8829978378241,12.1529255036342));
#4425=CARTESIAN_POINT('Ctrl Pts',(13.7872189777021,-26.0282054081263,11.5295040511826));
#4426=CARTESIAN_POINT('Ctrl Pts',(13.2477071858834,-25.6555960486084,11.1575129861594));
#4427=CARTESIAN_POINT('Ctrl Pts',(12.3467215172027,-25.2718905240171,10.6992796672134));
#4428=CARTESIAN_POINT('Ctrl Pts',(12.0307673583841,-25.172067656002,10.564392312562));
#4429=CARTESIAN_POINT('Ctrl Pts',(11.3750808674203,-25.0361359943163,10.372517968392));
#4430=CARTESIAN_POINT('Ctrl Pts',(11.0350345849277,-25.0000000000105,10.3166247903575));
#4431=CARTESIAN_POINT('Ctrl Pts',(10.3408569305139,-25.0000000000105,10.3166247903575));
#4432=CARTESIAN_POINT('Ctrl Pts',(10.0008106480213,-25.0361359943163,10.372517968392));
#4433=CARTESIAN_POINT('Ctrl Pts',(9.3451241570575,-25.172067656002,10.564392312562));
#4434=CARTESIAN_POINT('Ctrl Pts',(9.02916999823889,-25.2718905240171,10.6992796672134));
#4435=CARTESIAN_POINT('Ctrl Pts',(8.12818432955822,-25.6555960486084,11.1575129861594));
#4436=CARTESIAN_POINT('Ctrl Pts',(7.58867253773952,-26.0282054081263,11.5295040511826));
#4437=CARTESIAN_POINT('Ctrl Pts',(6.73388010804173,-26.8829978378241,12.1529255036342));
#4438=CARTESIAN_POINT('Ctrl Pts',(6.3523582813727,-27.4219616375112,12.4565421384626));
#4439=CARTESIAN_POINT('Ctrl Pts',(5.8286871768484,-28.6467782612166,12.8812351576426));
#4440=CARTESIAN_POINT('Ctrl Pts',(5.6879457577208,-29.3340326242477,13.0000000000021));
#4441=CARTESIAN_POINT('Ctrl Pts',(5.6879457577208,-30.6659673757733,13.0000000000021));
#4442=CARTESIAN_POINT('Ctrl Pts',(5.8286871768484,-31.3532217388044,12.8812351576426));
#4443=CARTESIAN_POINT('Ctrl Pts',(6.3523582813727,-32.5780383625099,12.4565421384626));
#4444=CARTESIAN_POINT('Ctrl Pts',(6.73388010804173,-33.1170021621969,12.1529255036342));
#4445=CARTESIAN_POINT('Ctrl Pts',(7.58867253773952,-33.9717945918947,11.5295040511826));
#4446=CARTESIAN_POINT('Ctrl Pts',(8.12818432955822,-34.3444039514126,11.1575129861594));
#4447=CARTESIAN_POINT('Ctrl Pts',(9.0291699982389,-34.7281094760039,10.6992796672134));
#4448=CARTESIAN_POINT('Ctrl Pts',(9.34512415705749,-34.8279323440191,10.564392312562));
#4449=CARTESIAN_POINT('Ctrl Pts',(10.0008106480213,-34.9638640057048,10.372517968392));
#4450=CARTESIAN_POINT('Ctrl Pts',(10.3408569305139,-35.0000000000105,10.3166247903575));
#4451=CARTESIAN_POINT('Ctrl Pts',(10.6879457577208,-35.0000000000105,10.3166247903575));
#4452=CARTESIAN_POINT('Origin',(10.6879457577208,-30.0000000000105,20.0000000000021));
#4453=CARTESIAN_POINT('',(10.6879457577208,-35.0000000000105,3.68337520964672));
#4454=CARTESIAN_POINT('',(15.6879457577208,-30.0000000000105,1.00000000000212));
#4455=CARTESIAN_POINT('Ctrl Pts',(10.6879457577208,-35.0000000000105,3.68337520964672));
#4456=CARTESIAN_POINT('Ctrl Pts',(10.3408569305139,-35.0000000000105,3.68337520964672));
#4457=CARTESIAN_POINT('Ctrl Pts',(10.0008106480213,-34.9638640057048,3.62748203161225));
#4458=CARTESIAN_POINT('Ctrl Pts',(9.3451241570575,-34.8279323440191,3.4356076874422));
#4459=CARTESIAN_POINT('Ctrl Pts',(9.02916999823889,-34.7281094760039,3.30072033279082));
#4460=CARTESIAN_POINT('Ctrl Pts',(8.12818432955822,-34.3444039514126,2.84248701384487));
#4461=CARTESIAN_POINT('Ctrl Pts',(7.58867253773952,-33.9717945918947,2.47049594882166));
#4462=CARTESIAN_POINT('Ctrl Pts',(6.73388010804173,-33.1170021621969,1.84707449637));
#4463=CARTESIAN_POINT('Ctrl Pts',(6.3523582813727,-32.5780383625099,1.54345786154165));
#4464=CARTESIAN_POINT('Ctrl Pts',(5.8286871768484,-31.3532217388044,1.1187648423616));
#4465=CARTESIAN_POINT('Ctrl Pts',(5.6879457577208,-30.6659673757733,1.00000000000212));
#4466=CARTESIAN_POINT('Ctrl Pts',(5.6879457577208,-29.3340326242477,1.00000000000212));
#4467=CARTESIAN_POINT('Ctrl Pts',(5.8286871768484,-28.6467782612166,1.1187648423616));
#4468=CARTESIAN_POINT('Ctrl Pts',(6.3523582813727,-27.4219616375112,1.54345786154165));
#4469=CARTESIAN_POINT('Ctrl Pts',(6.73388010804173,-26.8829978378241,1.84707449637));
#4470=CARTESIAN_POINT('Ctrl Pts',(7.58867253773952,-26.0282054081263,2.47049594882166));
#4471=CARTESIAN_POINT('Ctrl Pts',(8.12818432955822,-25.6555960486084,2.84248701384487));
#4472=CARTESIAN_POINT('Ctrl Pts',(9.02916999823889,-25.2718905240171,3.30072033279082));
#4473=CARTESIAN_POINT('Ctrl Pts',(9.3451241570575,-25.172067656002,3.4356076874422));
#4474=CARTESIAN_POINT('Ctrl Pts',(10.0008106480213,-25.0361359943163,3.62748203161225));
#4475=CARTESIAN_POINT('Ctrl Pts',(10.3408569305139,-25.0000000000105,3.68337520964672));
#4476=CARTESIAN_POINT('Ctrl Pts',(11.0350345849277,-25.0000000000105,3.68337520964672));
#4477=CARTESIAN_POINT('Ctrl Pts',(11.3750808674203,-25.0361359943163,3.62748203161225));
#4478=CARTESIAN_POINT('Ctrl Pts',(12.0307673583841,-25.172067656002,3.43560768744221));
#4479=CARTESIAN_POINT('Ctrl Pts',(12.3467215172027,-25.2718905240171,3.30072033279082));
#4480=CARTESIAN_POINT('Ctrl Pts',(13.2477071858834,-25.6555960486084,2.84248701384486));
#4481=CARTESIAN_POINT('Ctrl Pts',(13.7872189777021,-26.0282054081263,2.47049594882166));
#4482=CARTESIAN_POINT('Ctrl Pts',(14.6420114073999,-26.8829978378241,1.84707449637));
#4483=CARTESIAN_POINT('Ctrl Pts',(15.0235332340689,-27.4219616375112,1.54345786154165));
#4484=CARTESIAN_POINT('Ctrl Pts',(15.5472043385932,-28.6467782612166,1.1187648423616));
#4485=CARTESIAN_POINT('Ctrl Pts',(15.6879457577208,-29.3340326242477,1.00000000000212));
#4486=CARTESIAN_POINT('Ctrl Pts',(15.6879457577208,-30.0000000000105,1.00000000000212));
#4487=CARTESIAN_POINT('Ctrl Pts',(15.6879457577208,-30.0000000000105,1.00000000000212));
#4488=CARTESIAN_POINT('Ctrl Pts',(15.6879457577208,-30.6659673757733,1.00000000000212));
#4489=CARTESIAN_POINT('Ctrl Pts',(15.5472043385932,-31.3532217388044,1.1187648423616));
#4490=CARTESIAN_POINT('Ctrl Pts',(15.0235332340689,-32.5780383625098,1.54345786154165));
#4491=CARTESIAN_POINT('Ctrl Pts',(14.6420114073999,-33.1170021621969,1.84707449637));
#4492=CARTESIAN_POINT('Ctrl Pts',(13.7872189777021,-33.9717945918947,2.47049594882166));
#4493=CARTESIAN_POINT('Ctrl Pts',(13.2477071858834,-34.3444039514126,2.84248701384487));
#4494=CARTESIAN_POINT('Ctrl Pts',(12.3467215172027,-34.7281094760039,3.30072033279082));
#4495=CARTESIAN_POINT('Ctrl Pts',(12.0307673583841,-34.8279323440191,3.43560768744221));
#4496=CARTESIAN_POINT('Ctrl Pts',(11.3750808674203,-34.9638640057048,3.62748203161225));
#4497=CARTESIAN_POINT('Ctrl Pts',(11.0350345849277,-35.0000000000105,3.68337520964672));
#4498=CARTESIAN_POINT('Ctrl Pts',(10.6879457577208,-35.0000000000105,3.68337520964672));
#4499=CARTESIAN_POINT('',(15.6879457577208,-30.0000000000105,-5.99999999999788));
#4500=CARTESIAN_POINT('',(15.6879457577208,-30.0000000000105,20.0000000000021));
#4501=CARTESIAN_POINT('Origin',(10.6879457577208,-30.0000000000105,-5.99999999999788));
#4502=CARTESIAN_POINT('Origin',(-9.3120542422792,14.9999999999895,20.0000000000021));
#4503=CARTESIAN_POINT('',(-4.3120542422792,14.9999999999895,20.0000000000021));
#4504=CARTESIAN_POINT('Origin',(-9.3120542422792,14.9999999999895,20.0000000000021));
#4505=CARTESIAN_POINT('',(-4.3120542422792,14.9999999999895,14.0000000000021));
#4506=CARTESIAN_POINT('',(-4.3120542422792,14.9999999999895,20.0000000000021));
#4507=CARTESIAN_POINT('Origin',(-9.3120542422792,14.9999999999895,14.0000000000021));
#4508=CARTESIAN_POINT('Origin',(10.6879457577208,-75.0000000000105,20.0000000000021));
#4509=CARTESIAN_POINT('',(15.6879457577208,-75.0000000000105,20.0000000000021));
#4510=CARTESIAN_POINT('Origin',(10.6879457577208,-75.0000000000105,20.0000000000021));
#4511=CARTESIAN_POINT('',(15.6879457577208,-75.0000000000105,14.0000000000021));
#4512=CARTESIAN_POINT('',(15.6879457577208,-75.0000000000105,20.0000000000021));
#4513=CARTESIAN_POINT('Origin',(10.6879457577208,-75.0000000000105,14.0000000000021));
#4514=CARTESIAN_POINT('Origin',(29.,28.9999999999895,19.0000000000021));
#4515=CARTESIAN_POINT('',(30.,28.9999999999895,19.0000000000021));
#4516=CARTESIAN_POINT('',(29.,28.9999999999895,20.0000000000021));
#4517=CARTESIAN_POINT('Origin',(29.,28.9999999999895,19.0000000000021));
#4518=CARTESIAN_POINT('',(29.,29.9999999999895,19.0000000000021));
#4519=CARTESIAN_POINT('Origin',(29.,28.9999999999895,19.0000000000021));
#4520=CARTESIAN_POINT('Origin',(29.,28.9999999999895,19.0000000000021));
#4521=CARTESIAN_POINT('Origin',(29.,28.9999999999895,-5.99999999999788));
#4522=CARTESIAN_POINT('',(30.,28.9999999999895,4.00000000000212));
#4523=CARTESIAN_POINT('',(29.,29.9999999999895,4.00000000000212));
#4524=CARTESIAN_POINT('Origin',(29.,28.9999999999895,4.00000000000212));
#4525=CARTESIAN_POINT('',(29.,29.9999999999895,-5.99999999999788));
#4526=CARTESIAN_POINT('',(30.,28.9999999999895,-5.99999999999788));
#4527=CARTESIAN_POINT('Origin',(-49.,28.9999999999895,19.0000000000021));
#4528=CARTESIAN_POINT('',(-49.,29.9999999999895,19.0000000000021));
#4529=CARTESIAN_POINT('',(-49.,28.9999999999895,20.0000000000021));
#4530=CARTESIAN_POINT('Origin',(-49.,28.9999999999895,19.0000000000021));
#4531=CARTESIAN_POINT('',(-50.,28.9999999999895,19.0000000000021));
#4532=CARTESIAN_POINT('Origin',(-49.,28.9999999999895,19.0000000000021));
#4533=CARTESIAN_POINT('Origin',(-49.,28.9999999999895,19.0000000000021));
#4534=CARTESIAN_POINT('Origin',(-49.,28.9999999999895,-5.99999999999788));
#4535=CARTESIAN_POINT('',(-49.,29.9999999999895,4.00000000000212));
#4536=CARTESIAN_POINT('',(-50.,28.9999999999895,4.00000000000212));
#4537=CARTESIAN_POINT('Origin',(-49.,28.9999999999895,4.00000000000212));
#4538=CARTESIAN_POINT('',(-50.,28.9999999999895,-5.99999999999788));
#4539=CARTESIAN_POINT('',(-49.,29.9999999999895,-5.99999999999788));
#4540=CARTESIAN_POINT('Origin',(29.,-89.0000000000105,19.0000000000021));
#4541=CARTESIAN_POINT('',(29.,-90.0000000000105,19.0000000000021));
#4542=CARTESIAN_POINT('',(29.,-89.0000000000105,20.0000000000021));
#4543=CARTESIAN_POINT('Origin',(29.,-89.0000000000105,19.0000000000021));
#4544=CARTESIAN_POINT('',(30.,-89.0000000000105,19.0000000000021));
#4545=CARTESIAN_POINT('Origin',(29.,-89.0000000000105,19.0000000000021));
#4546=CARTESIAN_POINT('Origin',(29.,-89.0000000000105,19.0000000000021));
#4547=CARTESIAN_POINT('Origin',(29.,-89.0000000000105,-5.99999999999788));
#4548=CARTESIAN_POINT('',(29.,-90.0000000000105,4.00000000000212));
#4549=CARTESIAN_POINT('',(30.,-89.0000000000105,4.00000000000212));
#4550=CARTESIAN_POINT('Origin',(29.,-89.0000000000105,4.00000000000212));
#4551=CARTESIAN_POINT('',(30.,-89.0000000000105,-5.99999999999788));
#4552=CARTESIAN_POINT('',(29.,-90.0000000000105,-5.99999999999788));
#4553=CARTESIAN_POINT('Origin',(29.,-60.0000000000105,19.0000000000021));
#4554=CARTESIAN_POINT('',(29.,-60.0000000000105,20.0000000000021));
#4555=CARTESIAN_POINT('',(30.,-60.0000000000105,19.0000000000021));
#4556=CARTESIAN_POINT('Origin',(-49.,-89.0000000000105,19.0000000000021));
#4557=CARTESIAN_POINT('',(-50.,-89.0000000000105,19.0000000000021));
#4558=CARTESIAN_POINT('',(-49.,-89.0000000000105,20.0000000000021));
#4559=CARTESIAN_POINT('Origin',(-49.,-89.0000000000105,19.0000000000021));
#4560=CARTESIAN_POINT('',(-49.,-90.0000000000105,19.0000000000021));
#4561=CARTESIAN_POINT('Origin',(-49.,-89.0000000000105,19.0000000000021));
#4562=CARTESIAN_POINT('Origin',(-49.,-89.0000000000105,19.0000000000021));
#4563=CARTESIAN_POINT('Origin',(-49.,-89.0000000000105,-5.99999999999788));
#4564=CARTESIAN_POINT('',(-50.,-89.0000000000105,4.00000000000212));
#4565=CARTESIAN_POINT('',(-49.,-90.0000000000105,4.00000000000212));
#4566=CARTESIAN_POINT('Origin',(-49.,-89.0000000000105,4.00000000000212));
#4567=CARTESIAN_POINT('',(-49.,-90.0000000000105,-5.99999999999788));
#4568=CARTESIAN_POINT('',(-50.,-89.0000000000105,-5.99999999999788));
#4569=CARTESIAN_POINT('Origin',(-30.,-89.0000000000105,19.0000000000021));
#4570=CARTESIAN_POINT('',(-30.,-89.0000000000105,20.0000000000021));
#4571=CARTESIAN_POINT('',(-30.,-90.0000000000105,19.0000000000021));
#4572=CARTESIAN_POINT('Origin',(-49.,-1.05160324892495E-11,19.0000000000021));
#4573=CARTESIAN_POINT('',(-49.,-1.05160324892495E-11,20.0000000000021));
#4574=CARTESIAN_POINT('',(-50.,-1.05160324892495E-11,19.0000000000021));
#4575=CARTESIAN_POINT('Origin',(10.,28.9999999999895,19.0000000000021));
#4576=CARTESIAN_POINT('',(10.,28.9999999999895,20.0000000000021));
#4577=CARTESIAN_POINT('',(10.,29.9999999999895,19.0000000000021));
#4578=CARTESIAN_POINT('Origin',(30.,-90.0000000000105,-5.99999999999788));
#4579=CARTESIAN_POINT('',(30.,-81.0000000000105,4.00000000000212));
#4580=CARTESIAN_POINT('',(30.,-82.5000000000105,4.00000000000212));
#4581=CARTESIAN_POINT('',(30.,-81.0000000000105,14.0000000000021));
#4582=CARTESIAN_POINT('',(30.,-81.0000000000105,-0.999999999997885));
#4583=CARTESIAN_POINT('',(30.,-69.0000000000105,14.0000000000021));
#4584=CARTESIAN_POINT('',(30.,-82.5000000000105,14.0000000000021));
#4585=CARTESIAN_POINT('',(30.,-69.0000000000105,4.00000000000212));
#4586=CARTESIAN_POINT('',(30.,-69.0000000000105,-0.999999999997885));
#4587=CARTESIAN_POINT('',(30.,-60.0000000000105,4.00000000000212));
#4588=CARTESIAN_POINT('',(30.,-82.5000000000105,4.00000000000212));
#4589=CARTESIAN_POINT('',(30.,-60.0000000000105,-5.99999999999788));
#4590=CARTESIAN_POINT('',(30.,-60.0000000000105,-5.99999999999788));
#4591=CARTESIAN_POINT('',(30.,-1.05160324892495E-11,-5.99999999999788));
#4592=CARTESIAN_POINT('',(30.,29.9999999999895,-5.99999999999788));
#4593=CARTESIAN_POINT('',(30.,-1.05160324892495E-11,4.00000000000212));
#4594=CARTESIAN_POINT('',(30.,-1.05160324892495E-11,-5.99999999999788));
#4595=CARTESIAN_POINT('',(30.,8.99999999998949,4.00000000000212));
#4596=CARTESIAN_POINT('',(30.,-37.5000000000105,4.00000000000212));
#4597=CARTESIAN_POINT('',(30.,8.99999999998948,14.0000000000021));
#4598=CARTESIAN_POINT('',(30.,8.99999999998949,-0.999999999997885));
#4599=CARTESIAN_POINT('',(30.,20.9999999999895,14.0000000000021));
#4600=CARTESIAN_POINT('',(30.,-37.5000000000105,14.0000000000021));
#4601=CARTESIAN_POINT('',(30.,20.9999999999895,4.00000000000212));
#4602=CARTESIAN_POINT('',(30.,20.9999999999895,-0.999999999997885));
#4603=CARTESIAN_POINT('',(30.,-37.5000000000105,4.00000000000212));
#4604=CARTESIAN_POINT('',(30.,-24.0000000000105,7.00000000000211));
#4605=CARTESIAN_POINT('Origin',(30.,-30.0000000000105,7.00000000000211));
#4606=CARTESIAN_POINT('Origin',(-50.,-90.0000000000105,-5.99999999999788));
#4607=CARTESIAN_POINT('',(-30.,-90.0000000000105,4.00000000000212));
#4608=CARTESIAN_POINT('Origin',(-10.,-75.0000000000105,4.00000000000212));
#4609=CARTESIAN_POINT('',(-50.,-81.0000000000105,4.00000000000212));
#4610=CARTESIAN_POINT('',(-50.,-22.5000000000105,4.00000000000212));
#4611=CARTESIAN_POINT('',(-50.,-81.0000000000105,4.00000000000212));
#4612=CARTESIAN_POINT('Origin',(-10.,-30.0000000000105,20.0000000000021));
#4613=CARTESIAN_POINT('Origin',(70.,-30.0000000000105,7.00000000000211));
#4614=CARTESIAN_POINT('',(-50.,-24.0000000000105,7.00000000000211));
#4615=CARTESIAN_POINT('',(70.,-24.0000000000105,7.00000000000211));
#4616=CARTESIAN_POINT('Origin',(-50.,-30.0000000000105,7.00000000000211));
#4617=CARTESIAN_POINT('Origin',(-90.,8.99999999998948,4.00000000000212));
#4618=CARTESIAN_POINT('',(-50.,8.99999999998948,14.0000000000021));
#4619=CARTESIAN_POINT('',(-50.,8.99999999998948,4.00000000000212));
#4620=CARTESIAN_POINT('',(-50.,8.99999999998948,-0.999999999997885));
#4621=CARTESIAN_POINT('',(70.,8.99999999998948,14.0000000000021));
#4622=CARTESIAN_POINT('',(-50.,8.99999999998948,4.00000000000212));
#4623=CARTESIAN_POINT('Origin',(70.,20.9999999999895,4.00000000000212));
#4624=CARTESIAN_POINT('',(-50.,20.9999999999895,4.00000000000212));
#4625=CARTESIAN_POINT('',(-50.,20.9999999999895,14.0000000000021));
#4626=CARTESIAN_POINT('',(-50.,20.9999999999895,-0.999999999997885));
#4627=CARTESIAN_POINT('',(30.,20.9999999999895,4.00000000000212));
#4628=CARTESIAN_POINT('',(-90.,20.9999999999895,14.0000000000021));
#4629=CARTESIAN_POINT('Origin',(-10.,14.9999999999895,14.0000000000021));
#4630=CARTESIAN_POINT('',(-50.,22.4999999999895,14.0000000000021));
#4631=CARTESIAN_POINT('Origin',(-90.,-81.0000000000105,4.00000000000212));
#4632=CARTESIAN_POINT('',(-50.,-81.0000000000105,14.0000000000021));
#4633=CARTESIAN_POINT('',(-50.,-81.0000000000105,-0.999999999997885));
#4634=CARTESIAN_POINT('',(-90.,-81.0000000000105,14.0000000000021));
#4635=CARTESIAN_POINT('Origin',(70.,-69.0000000000105,4.00000000000212));
#4636=CARTESIAN_POINT('',(-50.,-69.0000000000105,4.00000000000212));
#4637=CARTESIAN_POINT('',(-50.,-69.0000000000105,14.0000000000021));
#4638=CARTESIAN_POINT('',(-50.,-69.0000000000105,-0.999999999997885));
#4639=CARTESIAN_POINT('',(30.,-69.0000000000105,4.00000000000212));
#4640=CARTESIAN_POINT('',(70.,-69.0000000000105,14.0000000000021));
#4641=CARTESIAN_POINT('Origin',(-10.,-75.0000000000105,14.0000000000021));
#4642=CARTESIAN_POINT('',(-50.,-22.5000000000105,14.0000000000021));
#4643=CARTESIAN_POINT('Origin',(-10.,14.9999999999895,4.00000000000212));
#4644=CARTESIAN_POINT('',(-50.,22.4999999999895,4.00000000000212));
#4645=CARTESIAN_POINT('',(10.,29.9999999999895,4.00000000000212));
#4646=CARTESIAN_POINT('Origin',(-10.,-75.0000000000105,4.00000000000212));
#4647=CARTESIAN_POINT('',(-50.,-60.0000000000105,4.00000000000212));
#4648=CARTESIAN_POINT('',(-50.,-22.5000000000105,4.00000000000212));
#4649=CARTESIAN_POINT('',(70.,-60.0000000000105,4.00000000000212));
#4650=CARTESIAN_POINT('Origin',(-10.,14.9999999999895,4.00000000000212));
#4651=CARTESIAN_POINT('',(-50.,-1.05160324892495E-11,4.00000000000212));
#4652=CARTESIAN_POINT('',(70.,-1.05160324892495E-11,4.00000000000212));
#4653=CARTESIAN_POINT('',(-50.,22.4999999999895,4.00000000000212));
#4654=CARTESIAN_POINT('Origin',(-90.,-1.05160324892495E-11,-5.99999999999788));
#4655=CARTESIAN_POINT('',(-50.,-1.05160324892495E-11,-5.99999999999788));
#4656=CARTESIAN_POINT('',(-50.,-1.05160324892495E-11,-5.99999999999788));
#4657=CARTESIAN_POINT('',(-50.,-1.05160324892495E-11,-5.99999999999788));
#4658=CARTESIAN_POINT('Origin',(70.,-60.0000000000105,-5.99999999999788));
#4659=CARTESIAN_POINT('',(-50.,-60.0000000000105,-5.99999999999788));
#4660=CARTESIAN_POINT('',(-50.,-60.0000000000105,-5.99999999999788));
#4661=CARTESIAN_POINT('',(30.,-60.0000000000105,-5.99999999999788));
#4662=CARTESIAN_POINT('Origin',(-50.,29.9999999999895,-5.99999999999788));
#4663=CARTESIAN_POINT('',(-50.,-90.0000000000105,-5.99999999999788));
#4664=CARTESIAN_POINT('Origin',(-10.,-30.0000000000105,-5.99999999999788));
#4665=CARTESIAN_POINT('Origin',(30.,29.9999999999895,-5.99999999999788));
#4666=CARTESIAN_POINT('',(0.,0.,0.));
#4667=CARTESIAN_POINT('Origin',(20.,59.9999999999895,2.1138646388863E-12));
#4668=CARTESIAN_POINT('',(85.,42.4999999999895,2.11172150698779E-12));
#4669=CARTESIAN_POINT('Origin',(85.,59.9999999999895,2.1138646388863E-12));
#4670=CARTESIAN_POINT('',(20.,42.4999999999895,2.11172150698779E-12));
#4671=CARTESIAN_POINT('',(20.,42.4999999999895,2.11172150698779E-12));
#4672=CARTESIAN_POINT('Origin',(20.,59.9999999999895,2.1138646388863E-12));
#4673=CARTESIAN_POINT('Origin',(85.,59.9999999999895,2.1138646388863E-12));
#4674=CARTESIAN_POINT('Origin',(-90.,84.9999999999895,-14.9999999999979));
#4675=CARTESIAN_POINT('',(20.,89.9999999999895,-9.99999999999789));
#4676=CARTESIAN_POINT('',(20.,79.9999999999895,-19.9999999999979));
#4677=CARTESIAN_POINT('',(20.,82.4999999999895,-17.4999999999979));
#4678=CARTESIAN_POINT('',(-90.,79.9999999999895,-19.9999999999979));
#4679=CARTESIAN_POINT('',(-90.,79.9999999999895,-19.9999999999979));
#4680=CARTESIAN_POINT('',(-90.,89.9999999999895,-9.99999999999789));
#4681=CARTESIAN_POINT('',(-90.,82.4999999999895,-17.4999999999979));
#4682=CARTESIAN_POINT('',(-90.,89.9999999999895,-9.99999999999789));
#4683=CARTESIAN_POINT('Origin',(-90.,59.9999999999895,2.11275441586167E-12));
#4684=CARTESIAN_POINT('',(-90.,39.9999999999895,-19.9999999999979));
#4685=CARTESIAN_POINT('',(-90.,89.9999999999895,-19.9999999999979));
#4686=CARTESIAN_POINT('',(-90.,29.9999999999895,-9.99999999999789));
#4687=CARTESIAN_POINT('',(-90.,37.4999999999895,-17.4999999999979));
#4688=CARTESIAN_POINT('',(-90.,29.9999999999895,10.0000000000021));
#4689=CARTESIAN_POINT('',(-90.,29.9999999999895,-19.9999999999979));
#4690=CARTESIAN_POINT('',(-90.,39.9999999999895,20.0000000000021));
#4691=CARTESIAN_POINT('',(-90.,37.4999999999895,17.5000000000021));
#4692=CARTESIAN_POINT('',(-90.,79.9999999999895,20.0000000000021));
#4693=CARTESIAN_POINT('',(-90.,29.9999999999895,20.0000000000021));
#4694=CARTESIAN_POINT('',(-90.,89.9999999999895,10.0000000000021));
#4695=CARTESIAN_POINT('',(-90.,82.4999999999895,17.5000000000021));
#4696=CARTESIAN_POINT('',(-90.,89.9999999999895,20.0000000000021));
#4697=CARTESIAN_POINT('Origin',(-90.,29.9999999999895,-19.9999999999979));
#4698=CARTESIAN_POINT('',(20.,39.9999999999895,-19.9999999999979));
#4699=CARTESIAN_POINT('',(20.,89.9999999999895,-19.9999999999979));
#4700=CARTESIAN_POINT('',(-90.,39.9999999999895,-19.9999999999979));
#4701=CARTESIAN_POINT('Origin',(-90.,34.9999999999895,-14.9999999999979));
#4702=CARTESIAN_POINT('',(20.,29.9999999999895,-9.99999999999789));
#4703=CARTESIAN_POINT('',(20.,37.4999999999895,-17.4999999999979));
#4704=CARTESIAN_POINT('',(-90.,29.9999999999895,-9.99999999999789));
#4705=CARTESIAN_POINT('Origin',(-90.,84.9999999999895,15.0000000000021));
#4706=CARTESIAN_POINT('',(20.,79.9999999999895,20.0000000000021));
#4707=CARTESIAN_POINT('',(20.,89.9999999999895,10.0000000000021));
#4708=CARTESIAN_POINT('',(20.,82.4999999999895,17.5000000000021));
#4709=CARTESIAN_POINT('',(-90.,89.9999999999895,10.0000000000021));
#4710=CARTESIAN_POINT('',(-90.,79.9999999999895,20.0000000000021));
#4711=CARTESIAN_POINT('Origin',(-90.,89.9999999999895,20.0000000000021));
#4712=CARTESIAN_POINT('',(20.,39.9999999999895,20.0000000000021));
#4713=CARTESIAN_POINT('',(-90.,39.9999999999895,20.0000000000021));
#4714=CARTESIAN_POINT('',(20.,29.9999999999895,20.0000000000021));
#4715=CARTESIAN_POINT('Origin',(-90.,34.9999999999895,15.0000000000021));
#4716=CARTESIAN_POINT('',(20.,29.9999999999895,10.0000000000021));
#4717=CARTESIAN_POINT('',(20.,37.4999999999895,17.5000000000021));
#4718=CARTESIAN_POINT('',(-90.,29.9999999999895,10.0000000000021));
#4719=CARTESIAN_POINT('Origin',(-90.,29.9999999999895,20.0000000000021));
#4720=CARTESIAN_POINT('',(20.,29.9999999999895,-19.9999999999979));
#4721=CARTESIAN_POINT('Origin',(-90.,89.9999999999895,-19.9999999999979));
#4722=CARTESIAN_POINT('',(20.,89.9999999999895,20.0000000000021));
#4723=CARTESIAN_POINT('Origin',(20.,59.9999999999895,2.11164419283705E-12));
#4724=CARTESIAN_POINT('',(0.,0.,0.));
#4725=CARTESIAN_POINT('Origin',(-90.,-30.0000000000105,7.00000000000211));
#4726=CARTESIAN_POINT('',(-80.,-23.0000000000105,7.00000000000211));
#4727=CARTESIAN_POINT('Origin',(-80.,-30.0000000000105,7.00000000000211));
#4728=CARTESIAN_POINT('',(-89.,-23.0000000000105,7.00000000000211));
#4729=CARTESIAN_POINT('',(-90.,-23.0000000000105,7.00000000000211));
#4730=CARTESIAN_POINT('Origin',(-89.,-30.0000000000105,7.00000000000211));
#4731=CARTESIAN_POINT('Origin',(-90.,-30.0000000000105,7.00000000000211));
#4732=CARTESIAN_POINT('',(-80.,-24.0000000000105,7.00000000000211));
#4733=CARTESIAN_POINT('Origin',(-80.,-30.0000000000105,7.00000000000211));
#4734=CARTESIAN_POINT('',(-90.,-24.0000000000105,7.00000000000211));
#4735=CARTESIAN_POINT('',(-90.,-24.0000000000105,7.00000000000211));
#4736=CARTESIAN_POINT('Origin',(-90.,-30.0000000000105,7.00000000000211));
#4737=CARTESIAN_POINT('Origin',(-80.,-30.0000000000105,7.00000000000211));
#4738=CARTESIAN_POINT('Origin',(-90.,-30.0000000000105,7.00000000000211));
#4739=CARTESIAN_POINT('',(-89.,-19.0000000000105,7.00000000000211));
#4740=CARTESIAN_POINT('Origin',(-89.,-30.0000000000105,7.00000000000211));
#4741=CARTESIAN_POINT('',(-90.,-19.0000000000105,7.00000000000211));
#4742=CARTESIAN_POINT('',(-90.,-19.0000000000105,7.00000000000211));
#4743=CARTESIAN_POINT('Origin',(-90.,-30.0000000000105,7.00000000000211));
#4744=CARTESIAN_POINT('Origin',(-89.,-30.0000000000105,7.00000000000211));
#4745=CARTESIAN_POINT('Origin',(-90.,-30.0000000000105,7.00000000000211));
#4746=CARTESIAN_POINT('',(0.,0.,0.));
#4747=CARTESIAN_POINT('Origin',(-110.,87.4999999999895,-17.4999999999979));
#4748=CARTESIAN_POINT('',(-90.,89.9999999999895,-14.9999999999979));
#4749=CARTESIAN_POINT('',(-90.,84.9999999999895,-19.9999999999979));
#4750=CARTESIAN_POINT('',(-90.,69.9999999999895,-34.9999999999979));
#4751=CARTESIAN_POINT('',(-110.,84.9999999999895,-19.9999999999979));
#4752=CARTESIAN_POINT('',(-110.,84.9999999999895,-19.9999999999979));
#4753=CARTESIAN_POINT('',(-110.,89.9999999999895,-14.9999999999979));
#4754=CARTESIAN_POINT('',(-110.,69.9999999999895,-34.9999999999979));
#4755=CARTESIAN_POINT('',(-110.,89.9999999999895,-14.9999999999979));
#4756=CARTESIAN_POINT('Origin',(-110.,-90.0000000000105,-19.9999999999979));
#4757=CARTESIAN_POINT('',(-90.,-85.0000000000105,-19.9999999999979));
#4758=CARTESIAN_POINT('',(-90.,-90.0000000000105,-19.9999999999979));
#4759=CARTESIAN_POINT('',(-110.,-85.0000000000105,-19.9999999999979));
#4760=CARTESIAN_POINT('',(-110.,-85.0000000000105,-19.9999999999979));
#4761=CARTESIAN_POINT('',(-110.,-90.0000000000105,-19.9999999999979));
#4762=CARTESIAN_POINT('Origin',(-90.,-1.05160324892495E-11,2.1138646388863E-12));
#4763=CARTESIAN_POINT('',(-90.,89.9999999999895,15.0000000000021));
#4764=CARTESIAN_POINT('',(-90.,89.9999999999895,-19.9999999999979));
#4765=CARTESIAN_POINT('',(-90.,84.9999999999895,20.0000000000021));
#4766=CARTESIAN_POINT('',(-90.,69.9999999999895,35.0000000000021));
#4767=CARTESIAN_POINT('',(-90.,-85.0000000000105,20.0000000000021));
#4768=CARTESIAN_POINT('',(-90.,89.9999999999895,20.0000000000021));
#4769=CARTESIAN_POINT('',(-90.,-90.0000000000105,15.0000000000021));
#4770=CARTESIAN_POINT('',(-90.,-70.0000000000105,35.0000000000021));
#4771=CARTESIAN_POINT('',(-90.,-90.0000000000105,-14.9999999999979));
#4772=CARTESIAN_POINT('',(-90.,-90.0000000000105,20.0000000000021));
#4773=CARTESIAN_POINT('',(-90.,-70.0000000000105,-34.9999999999979));
#4774=CARTESIAN_POINT('Origin',(-110.,-87.5000000000105,-17.4999999999979));
#4775=CARTESIAN_POINT('',(-110.,-90.0000000000105,-14.9999999999979));
#4776=CARTESIAN_POINT('',(-110.,-90.0000000000105,-14.9999999999979));
#4777=CARTESIAN_POINT('',(-110.,-70.0000000000105,-34.9999999999979));
#4778=CARTESIAN_POINT('Origin',(-110.,-90.0000000000105,20.0000000000021));
#4779=CARTESIAN_POINT('',(-110.,-90.0000000000105,15.0000000000021));
#4780=CARTESIAN_POINT('',(-110.,-90.0000000000105,15.0000000000021));
#4781=CARTESIAN_POINT('',(-110.,-90.0000000000105,20.0000000000021));
#4782=CARTESIAN_POINT('Origin',(-110.,87.4999999999895,17.5000000000021));
#4783=CARTESIAN_POINT('',(-110.,89.9999999999895,15.0000000000021));
#4784=CARTESIAN_POINT('',(-110.,89.9999999999895,15.0000000000021));
#4785=CARTESIAN_POINT('',(-110.,84.9999999999895,20.0000000000021));
#4786=CARTESIAN_POINT('',(-110.,69.9999999999895,35.0000000000021));
#4787=CARTESIAN_POINT('',(-110.,84.9999999999895,20.0000000000021));
#4788=CARTESIAN_POINT('Origin',(-110.,89.9999999999895,-19.9999999999979));
#4789=CARTESIAN_POINT('',(-110.,89.9999999999895,-19.9999999999979));
#4790=CARTESIAN_POINT('Origin',(-110.,-87.5000000000105,17.5000000000021));
#4791=CARTESIAN_POINT('',(-110.,-85.0000000000105,20.0000000000021));
#4792=CARTESIAN_POINT('',(-110.,-85.0000000000105,20.0000000000021));
#4793=CARTESIAN_POINT('',(-110.,-70.0000000000105,35.0000000000021));
#4794=CARTESIAN_POINT('Origin',(-110.,89.9999999999895,20.0000000000021));
#4795=CARTESIAN_POINT('',(-110.,89.9999999999895,20.0000000000021));
#4796=CARTESIAN_POINT('Origin',(-110.,-1.05160324892495E-11,2.11275441586167E-12));
#4797=CARTESIAN_POINT('',(0.,0.,0.));
#4798=CARTESIAN_POINT('',(0.,0.,0.));
#4799=CARTESIAN_POINT('',(0.,0.,0.));
#4800=CARTESIAN_POINT('',(0.,0.,0.));
#4801=CARTESIAN_POINT('',(0.,0.,0.));
#4802=CARTESIAN_POINT('',(0.,0.,0.));
#4803=CARTESIAN_POINT('',(0.,0.,0.));
#4804=CARTESIAN_POINT('',(0.,0.,0.));
#4805=CARTESIAN_POINT('',(0.,0.,0.));
#4806=CARTESIAN_POINT('',(0.,0.,0.));
#4807=CARTESIAN_POINT('',(2.75052545837645E-49,-4.44089209850063E-16,8.15320033709099E-17));
#4808=UNCERTAINTY_MEASURE_WITH_UNIT(LENGTH_MEASURE(0.01),#4834,
'DISTANCE_ACCURACY_VALUE',
'Maximum model space distance between geometric entities at asserted c
onnectivities');
#4809=UNCERTAINTY_MEASURE_WITH_UNIT(LENGTH_MEASURE(0.01),#4834,
'DISTANCE_ACCURACY_VALUE',
'Maximum model space distance between geometric entities at asserted c
onnectivities');
#4810=UNCERTAINTY_MEASURE_WITH_UNIT(LENGTH_MEASURE(0.01),#4834,
'DISTANCE_ACCURACY_VALUE',
'Maximum model space distance between geometric entities at asserted c
onnectivities');
#4811=UNCERTAINTY_MEASURE_WITH_UNIT(LENGTH_MEASURE(0.01),#4834,
'DISTANCE_ACCURACY_VALUE',
'Maximum model space distance between geometric entities at asserted c
onnectivities');
#4812=UNCERTAINTY_MEASURE_WITH_UNIT(LENGTH_MEASURE(0.01),#4834,
'DISTANCE_ACCURACY_VALUE',
'Maximum model space distance between geometric entities at asserted c
onnectivities');
#4813=UNCERTAINTY_MEASURE_WITH_UNIT(LENGTH_MEASURE(0.01),#4834,
'DISTANCE_ACCURACY_VALUE',
'Maximum model space distance between geometric entities at asserted c
onnectivities');
#4814=UNCERTAINTY_MEASURE_WITH_UNIT(LENGTH_MEASURE(0.01),#4834,
'DISTANCE_ACCURACY_VALUE',
'Maximum model space distance between geometric entities at asserted c
onnectivities');
#4815=UNCERTAINTY_MEASURE_WITH_UNIT(LENGTH_MEASURE(0.01),#4834,
'DISTANCE_ACCURACY_VALUE',
'Maximum model space distance between geometric entities at asserted c
onnectivities');
#4816=UNCERTAINTY_MEASURE_WITH_UNIT(LENGTH_MEASURE(0.01),#4834,
'DISTANCE_ACCURACY_VALUE',
'Maximum model space distance between geometric entities at asserted c
onnectivities');
#4817=UNCERTAINTY_MEASURE_WITH_UNIT(LENGTH_MEASURE(0.01),#4834,
'DISTANCE_ACCURACY_VALUE',
'Maximum model space distance between geometric entities at asserted c
onnectivities');
#4818=UNCERTAINTY_MEASURE_WITH_UNIT(LENGTH_MEASURE(0.01),#4834,
'DISTANCE_ACCURACY_VALUE',
'Maximum model space distance between geometric entities at asserted c
onnectivities');
#4819=UNCERTAINTY_MEASURE_WITH_UNIT(LENGTH_MEASURE(0.01),#4834,
'DISTANCE_ACCURACY_VALUE',
'Maximum model space distance between geometric entities at asserted c
onnectivities');
#4820=UNCERTAINTY_MEASURE_WITH_UNIT(LENGTH_MEASURE(0.01),#4834,
'DISTANCE_ACCURACY_VALUE',
'Maximum model space distance between geometric entities at asserted c
onnectivities');
#4821=(
GEOMETRIC_REPRESENTATION_CONTEXT(3)
GLOBAL_UNCERTAINTY_ASSIGNED_CONTEXT((#4808))
GLOBAL_UNIT_ASSIGNED_CONTEXT((#4834,#4836,#4837))
REPRESENTATION_CONTEXT('','3D')
);
#4822=(
GEOMETRIC_REPRESENTATION_CONTEXT(3)
GLOBAL_UNCERTAINTY_ASSIGNED_CONTEXT((#4809))
GLOBAL_UNIT_ASSIGNED_CONTEXT((#4834,#4836,#4837))
REPRESENTATION_CONTEXT('','3D')
);
#4823=(
GEOMETRIC_REPRESENTATION_CONTEXT(3)
GLOBAL_UNCERTAINTY_ASSIGNED_CONTEXT((#4810))
GLOBAL_UNIT_ASSIGNED_CONTEXT((#4834,#4836,#4837))
REPRESENTATION_CONTEXT('','3D')
);
#4824=(
GEOMETRIC_REPRESENTATION_CONTEXT(3)
GLOBAL_UNCERTAINTY_ASSIGNED_CONTEXT((#4811))
GLOBAL_UNIT_ASSIGNED_CONTEXT((#4834,#4836,#4837))
REPRESENTATION_CONTEXT('','3D')
);
#4825=(
GEOMETRIC_REPRESENTATION_CONTEXT(3)
GLOBAL_UNCERTAINTY_ASSIGNED_CONTEXT((#4812))
GLOBAL_UNIT_ASSIGNED_CONTEXT((#4834,#4836,#4837))
REPRESENTATION_CONTEXT('','3D')
);
#4826=(
GEOMETRIC_REPRESENTATION_CONTEXT(3)
GLOBAL_UNCERTAINTY_ASSIGNED_CONTEXT((#4813))
GLOBAL_UNIT_ASSIGNED_CONTEXT((#4834,#4836,#4837))
REPRESENTATION_CONTEXT('','3D')
);
#4827=(
GEOMETRIC_REPRESENTATION_CONTEXT(3)
GLOBAL_UNCERTAINTY_ASSIGNED_CONTEXT((#4814))
GLOBAL_UNIT_ASSIGNED_CONTEXT((#4834,#4836,#4837))
REPRESENTATION_CONTEXT('','3D')
);
#4828=(
GEOMETRIC_REPRESENTATION_CONTEXT(3)
GLOBAL_UNCERTAINTY_ASSIGNED_CONTEXT((#4815))
GLOBAL_UNIT_ASSIGNED_CONTEXT((#4834,#4836,#4837))
REPRESENTATION_CONTEXT('','3D')
);
#4829=(
GEOMETRIC_REPRESENTATION_CONTEXT(3)
GLOBAL_UNCERTAINTY_ASSIGNED_CONTEXT((#4816))
GLOBAL_UNIT_ASSIGNED_CONTEXT((#4834,#4836,#4837))
REPRESENTATION_CONTEXT('','3D')
);
#4830=(
GEOMETRIC_REPRESENTATION_CONTEXT(3)
GLOBAL_UNCERTAINTY_ASSIGNED_CONTEXT((#4817))
GLOBAL_UNIT_ASSIGNED_CONTEXT((#4834,#4836,#4837))
REPRESENTATION_CONTEXT('','3D')
);
#4831=(
GEOMETRIC_REPRESENTATION_CONTEXT(3)
GLOBAL_UNCERTAINTY_ASSIGNED_CONTEXT((#4818))
GLOBAL_UNIT_ASSIGNED_CONTEXT((#4834,#4836,#4837))
REPRESENTATION_CONTEXT('','3D')
);
#4832=(
GEOMETRIC_REPRESENTATION_CONTEXT(3)
GLOBAL_UNCERTAINTY_ASSIGNED_CONTEXT((#4819))
GLOBAL_UNIT_ASSIGNED_CONTEXT((#4834,#4836,#4837))
REPRESENTATION_CONTEXT('','3D')
);
#4833=(
GEOMETRIC_REPRESENTATION_CONTEXT(3)
GLOBAL_UNCERTAINTY_ASSIGNED_CONTEXT((#4820))
GLOBAL_UNIT_ASSIGNED_CONTEXT((#4834,#4836,#4837))
REPRESENTATION_CONTEXT('','3D')
);
#4834=(
LENGTH_UNIT()
NAMED_UNIT(*)
SI_UNIT(.MILLI.,.METRE.)
);
#4835=(
LENGTH_UNIT()
NAMED_UNIT(*)
SI_UNIT($,.METRE.)
);
#4836=(
NAMED_UNIT(*)
PLANE_ANGLE_UNIT()
SI_UNIT($,.RADIAN.)
);
#4837=(
NAMED_UNIT(*)
SI_UNIT($,.STERADIAN.)
SOLID_ANGLE_UNIT()
);
#4838=SHAPE_DEFINITION_REPRESENTATION(#4850,#4873);
#4839=SHAPE_DEFINITION_REPRESENTATION(#4851,#4874);
#4840=SHAPE_DEFINITION_REPRESENTATION(#4852,#4875);
#4841=SHAPE_DEFINITION_REPRESENTATION(#4853,#4876);
#4842=SHAPE_DEFINITION_REPRESENTATION(#4854,#4877);
#4843=SHAPE_DEFINITION_REPRESENTATION(#4855,#4878);
#4844=SHAPE_DEFINITION_REPRESENTATION(#4856,#4879);
#4845=SHAPE_DEFINITION_REPRESENTATION(#4857,#4880);
#4846=SHAPE_DEFINITION_REPRESENTATION(#4858,#4881);
#4847=SHAPE_DEFINITION_REPRESENTATION(#4859,#4882);
#4848=SHAPE_DEFINITION_REPRESENTATION(#4860,#4883);
#4849=SHAPE_DEFINITION_REPRESENTATION(#4861,#4884);
#4850=PRODUCT_DEFINITION_SHAPE('',$,#4886);
#4851=PRODUCT_DEFINITION_SHAPE('',$,#4887);
#4852=PRODUCT_DEFINITION_SHAPE('',$,#4888);
#4853=PRODUCT_DEFINITION_SHAPE('',$,#4889);
#4854=PRODUCT_DEFINITION_SHAPE('',$,#4890);
#4855=PRODUCT_DEFINITION_SHAPE('',$,#4891);
#4856=PRODUCT_DEFINITION_SHAPE('',$,#4892);
#4857=PRODUCT_DEFINITION_SHAPE('',$,#4893);
#4858=PRODUCT_DEFINITION_SHAPE('',$,#4894);
#4859=PRODUCT_DEFINITION_SHAPE('',$,#4895);
#4860=PRODUCT_DEFINITION_SHAPE('',$,#4896);
#4861=PRODUCT_DEFINITION_SHAPE('',$,#4897);
#4862=PRODUCT_DEFINITION_SHAPE($,$,#44);
#4863=PRODUCT_DEFINITION_SHAPE($,$,#45);
#4864=PRODUCT_DEFINITION_SHAPE($,$,#46);
#4865=PRODUCT_DEFINITION_SHAPE($,$,#47);
#4866=PRODUCT_DEFINITION_SHAPE($,$,#48);
#4867=PRODUCT_DEFINITION_SHAPE($,$,#49);
#4868=PRODUCT_DEFINITION_SHAPE($,$,#50);
#4869=PRODUCT_DEFINITION_SHAPE($,$,#51);
#4870=PRODUCT_DEFINITION_SHAPE($,$,#52);
#4871=PRODUCT_DEFINITION_SHAPE($,$,#53);
#4872=PRODUCT_DEFINITION_SHAPE($,$,#54);
#4873=SHAPE_REPRESENTATION('',(#2820,#3079,#3080,#3081,#3082,#3083,#3084,
#3085,#3086,#3087,#3088,#3089),#4821);
#4874=SHAPE_REPRESENTATION('',(#2821),#4822);
#4875=SHAPE_REPRESENTATION('',(#2852),#4823);
#4876=SHAPE_REPRESENTATION('',(#2883),#4824);
#4877=SHAPE_REPRESENTATION('',(#2889),#4825);
#4878=SHAPE_REPRESENTATION('',(#2916),#4826);
#4879=SHAPE_REPRESENTATION('',(#2945),#4827);
#4880=SHAPE_REPRESENTATION('',(#2958),#4828);
#4881=SHAPE_REPRESENTATION('',(#2970),#4829);
#4882=SHAPE_REPRESENTATION('',(#3040),#4830);
#4883=SHAPE_REPRESENTATION('',(#3055),#4831);
#4884=SHAPE_REPRESENTATION('',(#3068),#4832);
#4885=PRODUCT_DEFINITION_CONTEXT('part definition',#4923,'design');
#4886=PRODUCT_DEFINITION('MAS-269','MAS-269',#4898,#4885);
#4887=PRODUCT_DEFINITION('Guide_Rail_01','Guide_Rail_01',#4899,#4885);
#4888=PRODUCT_DEFINITION('Guide_Rail_02','Guide_Rail_02',#4900,#4885);
#4889=PRODUCT_DEFINITION('Rod','Rod',#4901,#4885);
#4890=PRODUCT_DEFINITION('Front_Block','Front_Block',#4902,#4885);
#4891=PRODUCT_DEFINITION('Support_Block','Support_Block',#4903,#4885);
#4892=PRODUCT_DEFINITION('Rod_Mount_01','Rod_Mount_01',#4904,#4885);
#4893=PRODUCT_DEFINITION('Base','Base',#4905,#4885);
#4894=PRODUCT_DEFINITION('Top_Block','Top_Block',#4906,#4885);
#4895=PRODUCT_DEFINITION('Motor','Motor',#4907,#4885);
#4896=PRODUCT_DEFINITION('Rod_Mount_02','Rod_Mount_02',#4908,#4885);
#4897=PRODUCT_DEFINITION('Back_Block','Back_Block',#4909,#4885);
#4898=PRODUCT_DEFINITION_FORMATION('',$,#4925);
#4899=PRODUCT_DEFINITION_FORMATION('',$,#4926);
#4900=PRODUCT_DEFINITION_FORMATION('',$,#4927);
#4901=PRODUCT_DEFINITION_FORMATION('',$,#4928);
#4902=PRODUCT_DEFINITION_FORMATION('',$,#4929);
#4903=PRODUCT_DEFINITION_FORMATION('',$,#4930);
#4904=PRODUCT_DEFINITION_FORMATION('',$,#4931);
#4905=PRODUCT_DEFINITION_FORMATION('',$,#4932);
#4906=PRODUCT_DEFINITION_FORMATION('',$,#4933);
#4907=PRODUCT_DEFINITION_FORMATION('',$,#4934);
#4908=PRODUCT_DEFINITION_FORMATION('',$,#4935);
#4909=PRODUCT_DEFINITION_FORMATION('',$,#4936);
#4910=PRODUCT_RELATED_PRODUCT_CATEGORY('MAS-269','MAS-269',(#4925));
#4911=PRODUCT_RELATED_PRODUCT_CATEGORY('Guide_Rail_01','Guide_Rail_01',
(#4926));
#4912=PRODUCT_RELATED_PRODUCT_CATEGORY('Guide_Rail_02','Guide_Rail_02',
(#4927));
#4913=PRODUCT_RELATED_PRODUCT_CATEGORY('Rod','Rod',(#4928));
#4914=PRODUCT_RELATED_PRODUCT_CATEGORY('Front_Block','Front_Block',(#4929));
#4915=PRODUCT_RELATED_PRODUCT_CATEGORY('Support_Block','Support_Block',
(#4930));
#4916=PRODUCT_RELATED_PRODUCT_CATEGORY('Rod_Mount_01','Rod_Mount_01',(#4931));
#4917=PRODUCT_RELATED_PRODUCT_CATEGORY('Base','Base',(#4932));
#4918=PRODUCT_RELATED_PRODUCT_CATEGORY('Top_Block','Top_Block',(#4933));
#4919=PRODUCT_RELATED_PRODUCT_CATEGORY('Motor','Motor',(#4934));
#4920=PRODUCT_RELATED_PRODUCT_CATEGORY('Rod_Mount_02','Rod_Mount_02',(#4935));
#4921=PRODUCT_RELATED_PRODUCT_CATEGORY('Back_Block','Back_Block',(#4936));
#4922=APPLICATION_PROTOCOL_DEFINITION('international standard',
'automotive_design',2009,#4923);
#4923=APPLICATION_CONTEXT(
'Core Data for Automotive Mechanical Design Process');
#4924=PRODUCT_CONTEXT('part definition',#4923,'mechanical');
#4925=PRODUCT('MAS-269','MAS-269',$,(#4924));
#4926=PRODUCT('Guide_Rail_01','Guide_Rail_01',$,(#4924));
#4927=PRODUCT('Guide_Rail_02','Guide_Rail_02',$,(#4924));
#4928=PRODUCT('Rod','Rod',$,(#4924));
#4929=PRODUCT('Front_Block','Front_Block',$,(#4924));
#4930=PRODUCT('Support_Block','Support_Block',$,(#4924));
#4931=PRODUCT('Rod_Mount_01','Rod_Mount_01',$,(#4924));
#4932=PRODUCT('Base','Base',$,(#4924));
#4933=PRODUCT('Top_Block','Top_Block',$,(#4924));
#4934=PRODUCT('Motor','Motor',$,(#4924));
#4935=PRODUCT('Rod_Mount_02','Rod_Mount_02',$,(#4924));
#4936=PRODUCT('Back_Block','Back_Block',$,(#4924));
#4937=PRESENTATION_STYLE_ASSIGNMENT((#4941));
#4938=PRESENTATION_STYLE_ASSIGNMENT((#4942));
#4939=PRESENTATION_STYLE_ASSIGNMENT((#4943));
#4940=PRESENTATION_STYLE_ASSIGNMENT((#4944));
#4941=SURFACE_STYLE_USAGE(.BOTH.,#4945);
#4942=SURFACE_STYLE_USAGE(.BOTH.,#4946);
#4943=SURFACE_STYLE_USAGE(.BOTH.,#4947);
#4944=SURFACE_STYLE_USAGE(.BOTH.,#4948);
#4945=SURFACE_SIDE_STYLE('',(#4949));
#4946=SURFACE_SIDE_STYLE('',(#4950));
#4947=SURFACE_SIDE_STYLE('',(#4951));
#4948=SURFACE_SIDE_STYLE('',(#4952));
#4949=SURFACE_STYLE_FILL_AREA(#4953);
#4950=SURFACE_STYLE_FILL_AREA(#4954);
#4951=SURFACE_STYLE_FILL_AREA(#4955);
#4952=SURFACE_STYLE_FILL_AREA(#4956);
#4953=FILL_AREA_STYLE('Steel - Satin',(#4957));
#4954=FILL_AREA_STYLE('Steel - Satin (1)',(#4958));
#4955=FILL_AREA_STYLE('Steel - Satin',(#4959));
#4956=FILL_AREA_STYLE('Steel - Satin (1) (1)',(#4960));
#4957=FILL_AREA_STYLE_COLOUR('Steel - Satin',#4961);
#4958=FILL_AREA_STYLE_COLOUR('Steel - Satin (1)',#4962);
#4959=FILL_AREA_STYLE_COLOUR('Steel - Satin',#4963);
#4960=FILL_AREA_STYLE_COLOUR('Steel - Satin (1) (1)',#4964);
#4961=COLOUR_RGB('Steel - Satin',0.627450980392157,0.627450980392157,0.627450980392157);
#4962=COLOUR_RGB('Steel - Satin (1)',1.,0.823529411764706,0.823529411764706);
#4963=COLOUR_RGB('Steel - Satin',0.419607843137255,0.419607843137255,0.419607843137255);
#4964=COLOUR_RGB('Steel - Satin (1) (1)',0.447058823529412,0.623529411764706,
1.);
#4965=COLOUR_RGB('Dark Blue',0.08,0.2,0.34);
#4966=FILL_AREA_STYLE_COLOUR('',#4965);
#4967=FILL_AREA_STYLE('',(#4966));
#4968=SURFACE_STYLE_FILL_AREA(#4967);
#4969=SURFACE_SIDE_STYLE('',(#4968));
#4970=SURFACE_STYLE_USAGE(.BOTH.,#4969);
#4971=PRESENTATION_STYLE_ASSIGNMENT((#4970));
#4972=COLOUR_RGB('Light Blue',0.38,0.62,0.78);
#4973=FILL_AREA_STYLE_COLOUR('',#4972);
#4974=FILL_AREA_STYLE('',(#4973));
#4975=SURFACE_STYLE_FILL_AREA(#4974);
#4976=SURFACE_SIDE_STYLE('',(#4975));
#4977=SURFACE_STYLE_USAGE(.BOTH.,#4976);
#4978=PRESENTATION_STYLE_ASSIGNMENT((#4977));
#4979=COLOUR_RGB('Sky Blue',0.24,0.69,0.87);
#4980=FILL_AREA_STYLE_COLOUR('',#4979);
#4981=FILL_AREA_STYLE('',(#4980));
#4982=SURFACE_STYLE_FILL_AREA(#4981);
#4983=SURFACE_SIDE_STYLE('',(#4982));
#4984=SURFACE_STYLE_USAGE(.BOTH.,#4983);
#4985=PRESENTATION_STYLE_ASSIGNMENT((#4984));
#4986=COLOUR_RGB('Grey',0.48,0.52,0.57);
#4987=FILL_AREA_STYLE_COLOUR('',#4986);
#4988=FILL_AREA_STYLE('',(#4987));
#4989=SURFACE_STYLE_FILL_AREA(#4988);
#4990=SURFACE_SIDE_STYLE('',(#4989));
#4991=SURFACE_STYLE_USAGE(.BOTH.,#4990);
#4992=PRESENTATION_STYLE_ASSIGNMENT((#4991));
#4993=COLOUR_RGB('Black',0.12,0.14,0.17);
#4994=FILL_AREA_STYLE_COLOUR('',#4993);
#4995=FILL_AREA_STYLE('',(#4994));
#4996=SURFACE_STYLE_FILL_AREA(#4995);
#4997=SURFACE_SIDE_STYLE('',(#4996));
#4998=SURFACE_STYLE_USAGE(.BOTH.,#4997);
#4999=PRESENTATION_STYLE_ASSIGNMENT((#4998));
#5000=COLOUR_RGB('Off White',0.89,0.88,0.83);
#5001=FILL_AREA_STYLE_COLOUR('',#5000);
#5002=FILL_AREA_STYLE('',(#5001));
#5003=SURFACE_STYLE_FILL_AREA(#5002);
#5004=SURFACE_SIDE_STYLE('',(#5003));
#5005=SURFACE_STYLE_USAGE(.BOTH.,#5004);
#5006=PRESENTATION_STYLE_ASSIGNMENT((#5005));
ENDSEC;
END-ISO-10303-21;
